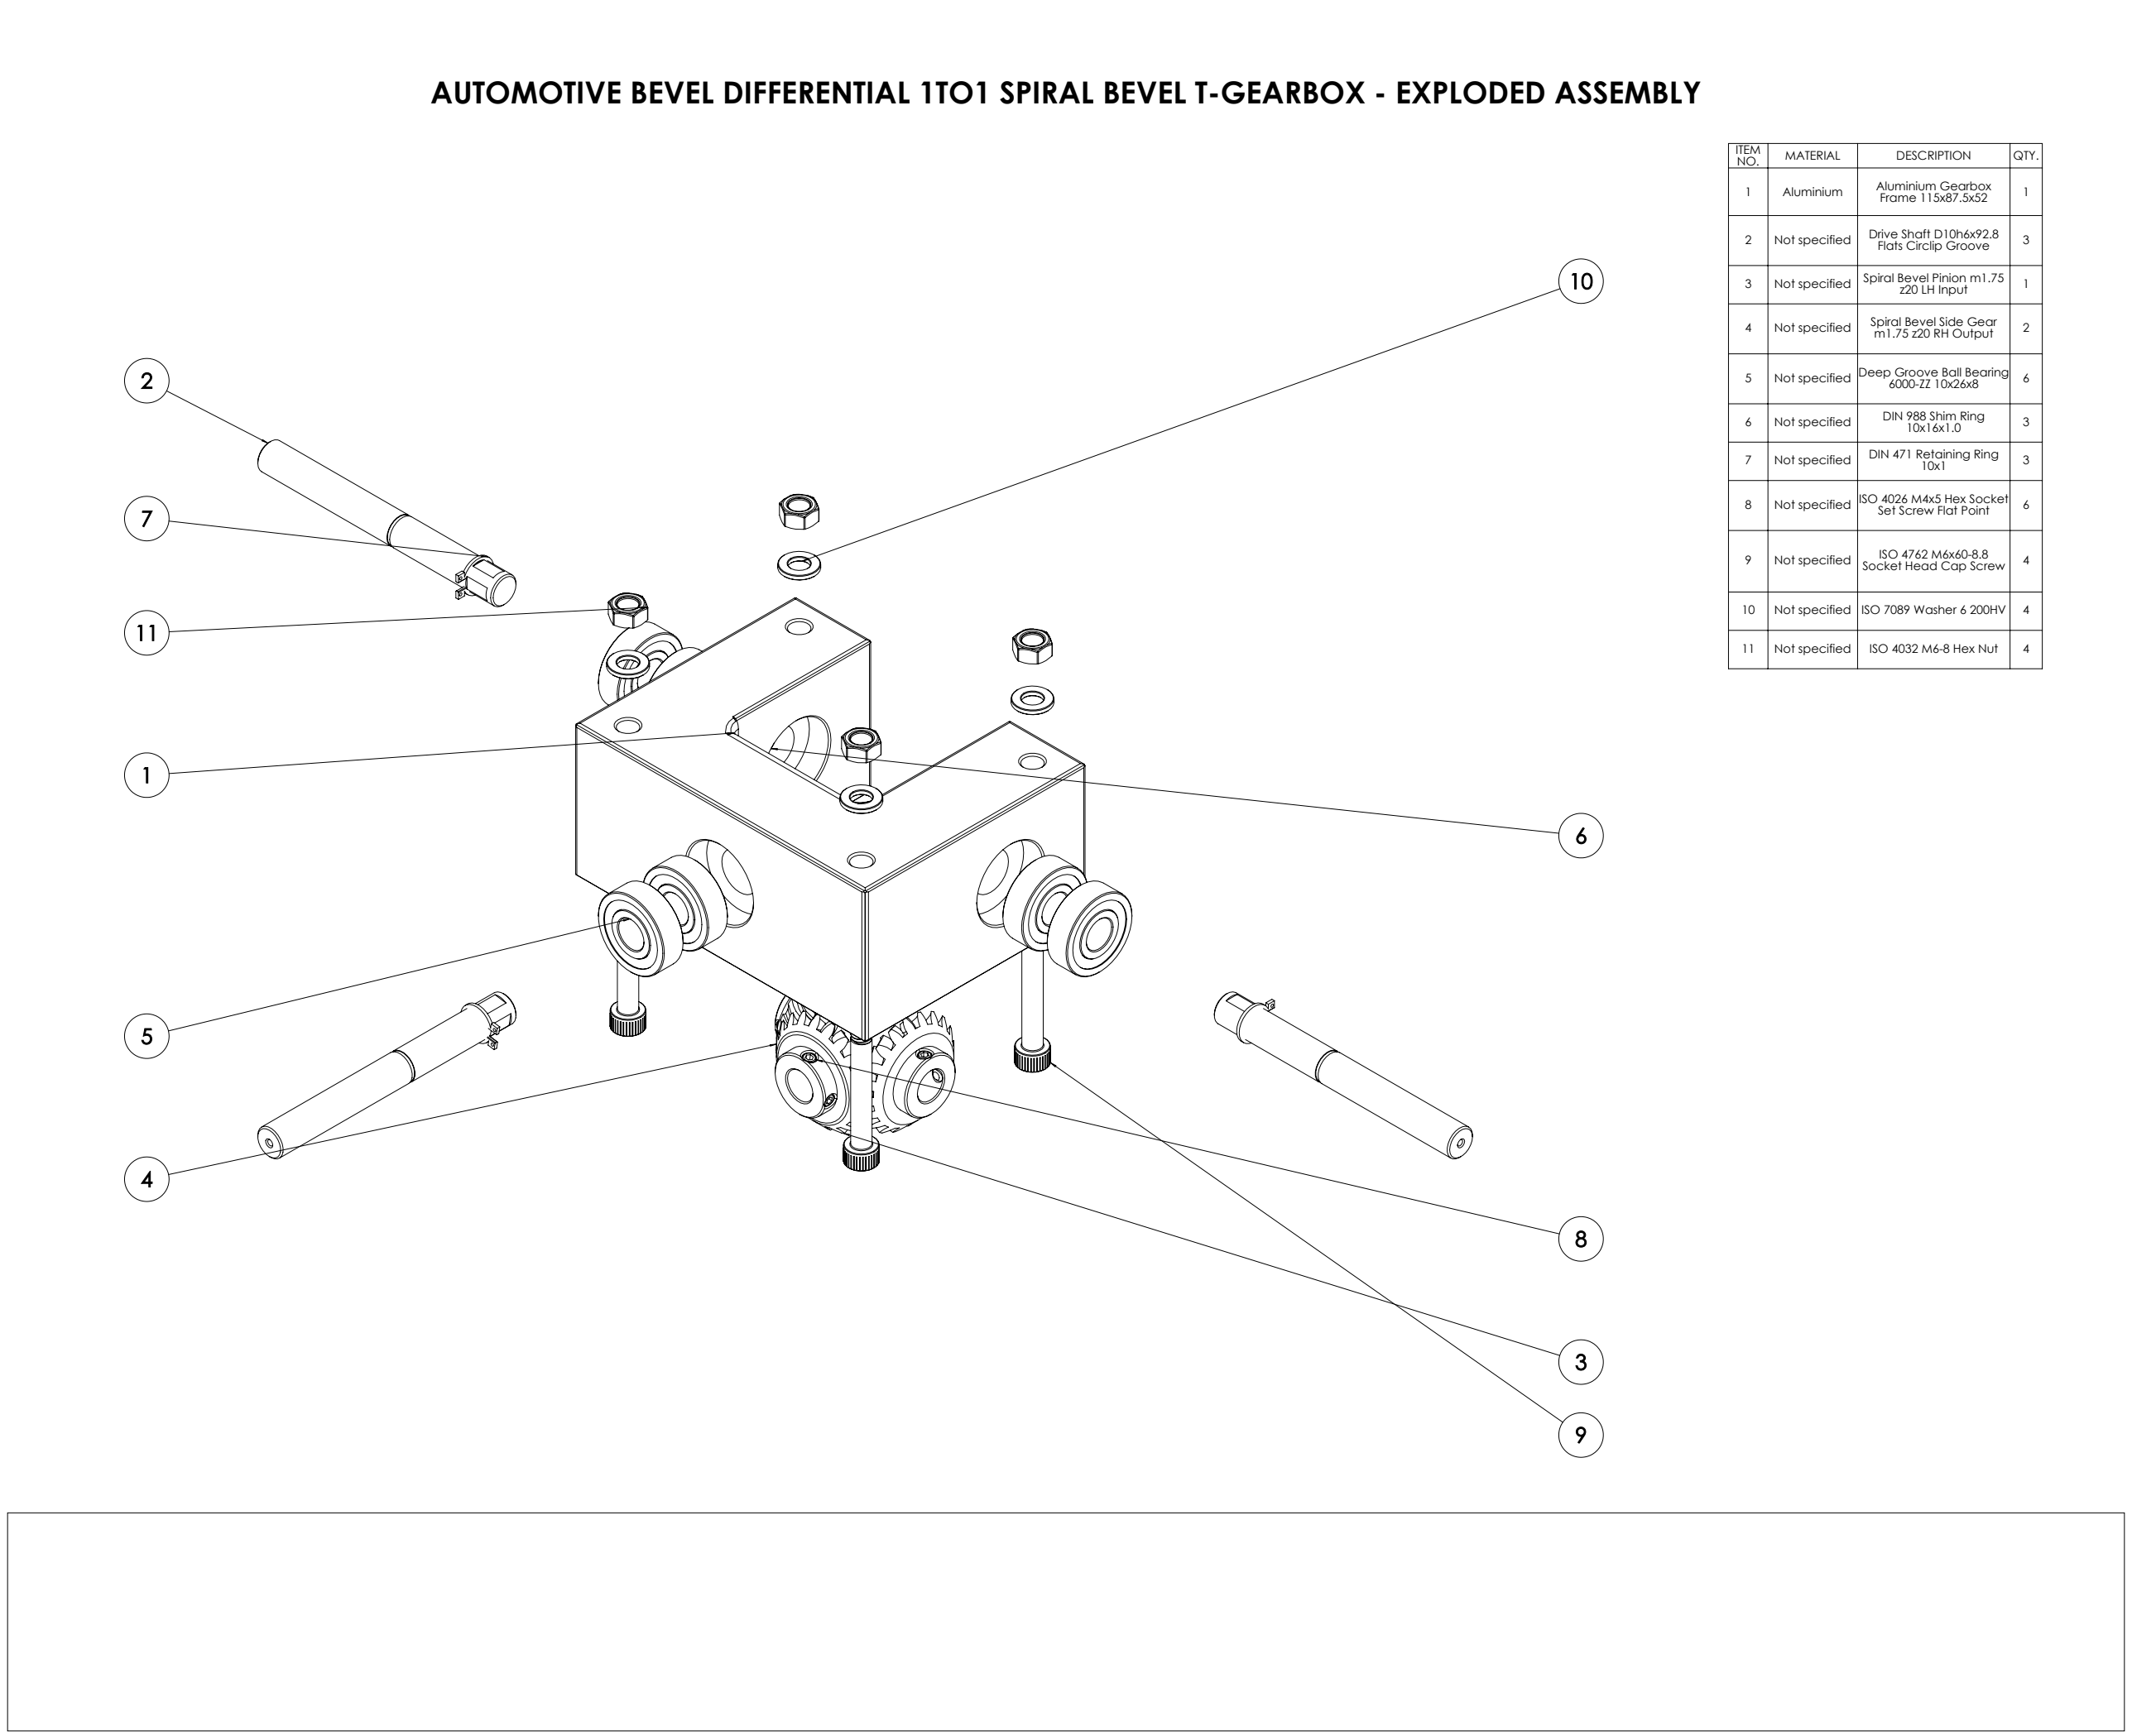
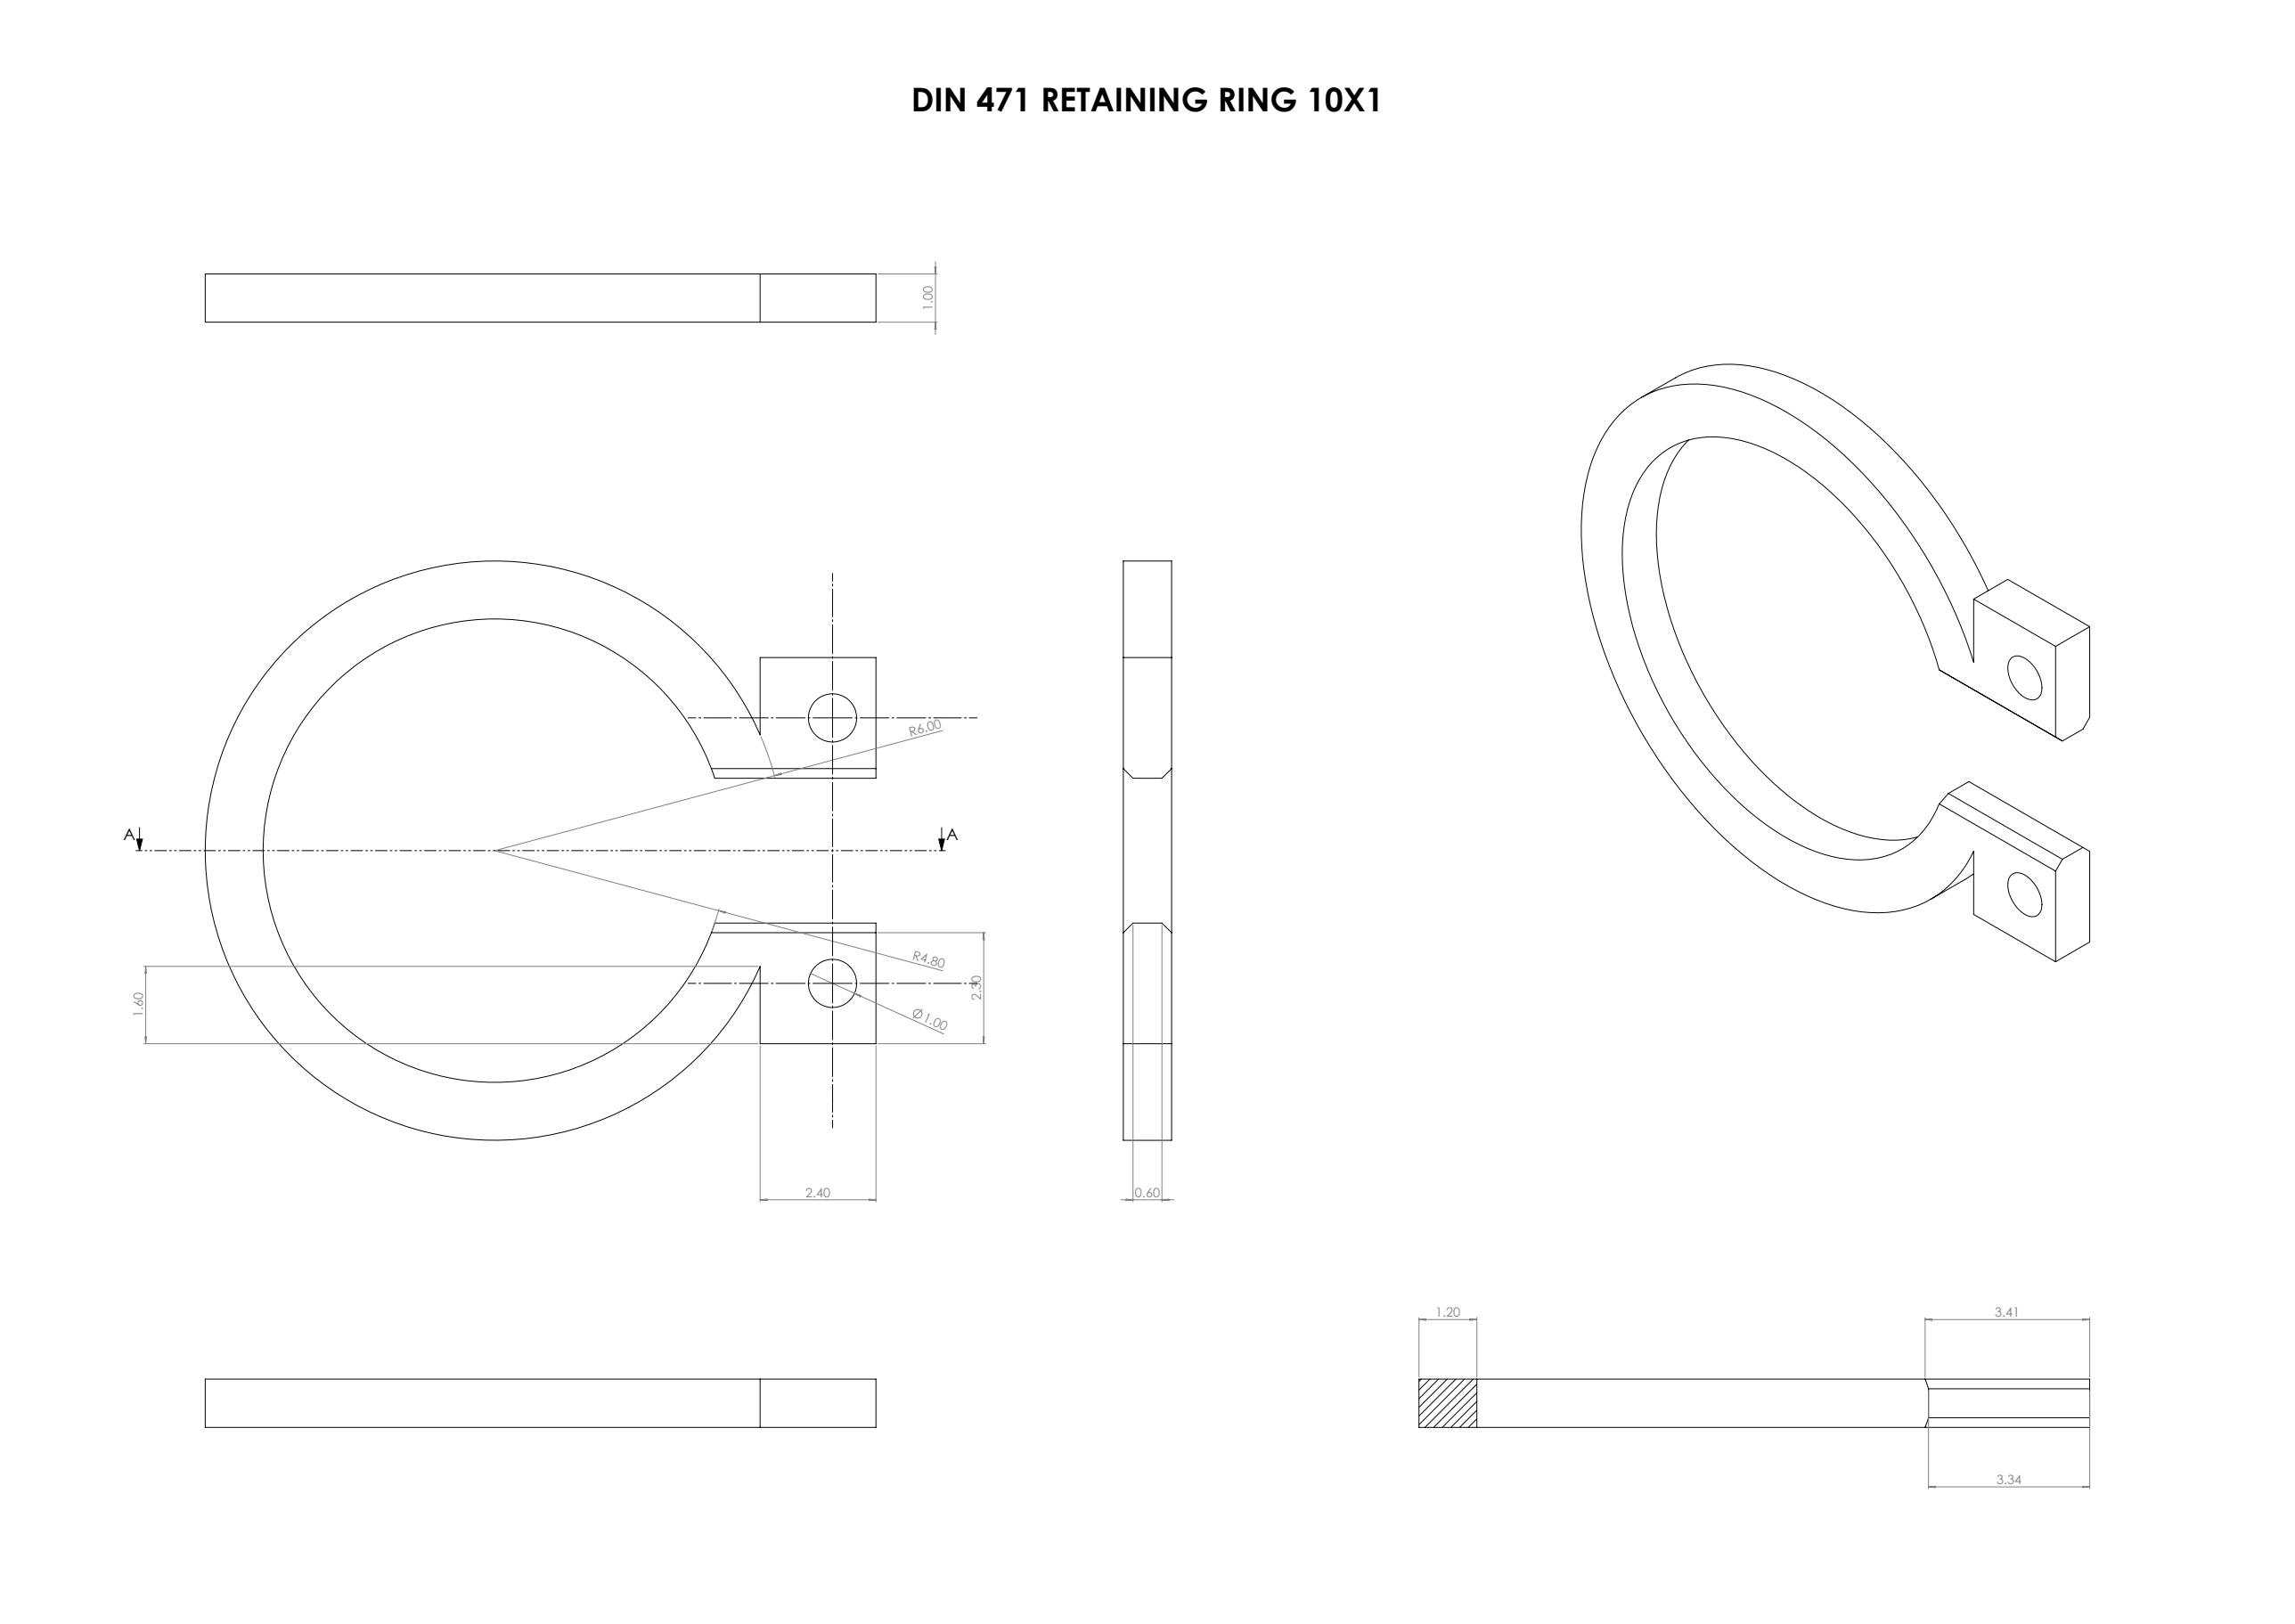
ISO-10303-21;
HEADER;
/* Generated by software containing ST-Developer
 * from STEP Tools, Inc. (www.steptools.com) 
 */

FILE_DESCRIPTION(
/* description */ (''),
/* implementation_level */ '2;1');

FILE_NAME(
/* name */ 
'MAS-358',
/* time_stamp */ '2026-10-22T00:21:42-07:00',
/* author */ (''),
/* organization */ (''),
/* preprocessor_version */ 'ST-DEVELOPER v20.2',
/* originating_system */ 'Autodesk Translation Framework v15.15.0.0',
/* authorisation */ '');

FILE_SCHEMA (('AUTOMOTIVE_DESIGN { 1 0 10303 214 3 1 1 }'));
ENDSEC;

DATA;
#10=MECHANICAL_DESIGN_GEOMETRIC_PRESENTATION_REPRESENTATION('',(#205,#206,
#207,#208,#209,#210,#211,#212,#213,#214,#215),#31638);
#11=ITEM_DEFINED_TRANSFORMATION($,$,#12614,#13583);
#12=ITEM_DEFINED_TRANSFORMATION($,$,#12865,#13584);
#13=ITEM_DEFINED_TRANSFORMATION($,$,#12776,#13585);
#14=ITEM_DEFINED_TRANSFORMATION($,$,#12900,#13586);
#15=ITEM_DEFINED_TRANSFORMATION($,$,#12986,#13587);
#16=ITEM_DEFINED_TRANSFORMATION($,$,#13096,#13588);
#17=ITEM_DEFINED_TRANSFORMATION($,$,#13105,#13589);
#18=ITEM_DEFINED_TRANSFORMATION($,$,#13136,#13590);
#19=ITEM_DEFINED_TRANSFORMATION($,$,#13175,#13591);
#20=ITEM_DEFINED_TRANSFORMATION($,$,#13515,#13592);
#21=ITEM_DEFINED_TRANSFORMATION($,$,#13535,#13593);
#22=ITEM_DEFINED_TRANSFORMATION($,$,#12865,#13594);
#23=ITEM_DEFINED_TRANSFORMATION($,$,#12865,#13595);
#24=ITEM_DEFINED_TRANSFORMATION($,$,#12900,#13596);
#25=ITEM_DEFINED_TRANSFORMATION($,$,#12986,#13597);
#26=ITEM_DEFINED_TRANSFORMATION($,$,#12986,#13598);
#27=ITEM_DEFINED_TRANSFORMATION($,$,#12986,#13599);
#28=ITEM_DEFINED_TRANSFORMATION($,$,#12986,#13600);
#29=ITEM_DEFINED_TRANSFORMATION($,$,#12986,#13601);
#30=ITEM_DEFINED_TRANSFORMATION($,$,#13096,#13602);
#31=ITEM_DEFINED_TRANSFORMATION($,$,#13096,#13603);
#32=ITEM_DEFINED_TRANSFORMATION($,$,#13105,#13604);
#33=ITEM_DEFINED_TRANSFORMATION($,$,#13105,#13605);
#34=ITEM_DEFINED_TRANSFORMATION($,$,#13136,#13606);
#35=ITEM_DEFINED_TRANSFORMATION($,$,#13136,#13607);
#36=ITEM_DEFINED_TRANSFORMATION($,$,#13136,#13608);
#37=ITEM_DEFINED_TRANSFORMATION($,$,#13136,#13609);
#38=ITEM_DEFINED_TRANSFORMATION($,$,#13136,#13610);
#39=ITEM_DEFINED_TRANSFORMATION($,$,#13175,#13611);
#40=ITEM_DEFINED_TRANSFORMATION($,$,#13175,#13612);
#41=ITEM_DEFINED_TRANSFORMATION($,$,#13175,#13613);
#42=ITEM_DEFINED_TRANSFORMATION($,$,#13515,#13614);
#43=ITEM_DEFINED_TRANSFORMATION($,$,#13515,#13615);
#44=ITEM_DEFINED_TRANSFORMATION($,$,#13515,#13616);
#45=ITEM_DEFINED_TRANSFORMATION($,$,#13535,#13617);
#46=ITEM_DEFINED_TRANSFORMATION($,$,#13535,#13618);
#47=ITEM_DEFINED_TRANSFORMATION($,$,#13535,#13619);
#48=(
REPRESENTATION_RELATIONSHIP($,$,#31705,#31704)
REPRESENTATION_RELATIONSHIP_WITH_TRANSFORMATION(#11)
SHAPE_REPRESENTATION_RELATIONSHIP()
);
#49=(
REPRESENTATION_RELATIONSHIP($,$,#31707,#31704)
REPRESENTATION_RELATIONSHIP_WITH_TRANSFORMATION(#12)
SHAPE_REPRESENTATION_RELATIONSHIP()
);
#50=(
REPRESENTATION_RELATIONSHIP($,$,#31706,#31704)
REPRESENTATION_RELATIONSHIP_WITH_TRANSFORMATION(#13)
SHAPE_REPRESENTATION_RELATIONSHIP()
);
#51=(
REPRESENTATION_RELATIONSHIP($,$,#31708,#31704)
REPRESENTATION_RELATIONSHIP_WITH_TRANSFORMATION(#14)
SHAPE_REPRESENTATION_RELATIONSHIP()
);
#52=(
REPRESENTATION_RELATIONSHIP($,$,#31709,#31704)
REPRESENTATION_RELATIONSHIP_WITH_TRANSFORMATION(#15)
SHAPE_REPRESENTATION_RELATIONSHIP()
);
#53=(
REPRESENTATION_RELATIONSHIP($,$,#31710,#31704)
REPRESENTATION_RELATIONSHIP_WITH_TRANSFORMATION(#16)
SHAPE_REPRESENTATION_RELATIONSHIP()
);
#54=(
REPRESENTATION_RELATIONSHIP($,$,#31711,#31704)
REPRESENTATION_RELATIONSHIP_WITH_TRANSFORMATION(#17)
SHAPE_REPRESENTATION_RELATIONSHIP()
);
#55=(
REPRESENTATION_RELATIONSHIP($,$,#31712,#31704)
REPRESENTATION_RELATIONSHIP_WITH_TRANSFORMATION(#18)
SHAPE_REPRESENTATION_RELATIONSHIP()
);
#56=(
REPRESENTATION_RELATIONSHIP($,$,#31713,#31704)
REPRESENTATION_RELATIONSHIP_WITH_TRANSFORMATION(#19)
SHAPE_REPRESENTATION_RELATIONSHIP()
);
#57=(
REPRESENTATION_RELATIONSHIP($,$,#31714,#31704)
REPRESENTATION_RELATIONSHIP_WITH_TRANSFORMATION(#20)
SHAPE_REPRESENTATION_RELATIONSHIP()
);
#58=(
REPRESENTATION_RELATIONSHIP($,$,#31715,#31704)
REPRESENTATION_RELATIONSHIP_WITH_TRANSFORMATION(#21)
SHAPE_REPRESENTATION_RELATIONSHIP()
);
#59=(
REPRESENTATION_RELATIONSHIP($,$,#31707,#31704)
REPRESENTATION_RELATIONSHIP_WITH_TRANSFORMATION(#22)
SHAPE_REPRESENTATION_RELATIONSHIP()
);
#60=(
REPRESENTATION_RELATIONSHIP($,$,#31707,#31704)
REPRESENTATION_RELATIONSHIP_WITH_TRANSFORMATION(#23)
SHAPE_REPRESENTATION_RELATIONSHIP()
);
#61=(
REPRESENTATION_RELATIONSHIP($,$,#31708,#31704)
REPRESENTATION_RELATIONSHIP_WITH_TRANSFORMATION(#24)
SHAPE_REPRESENTATION_RELATIONSHIP()
);
#62=(
REPRESENTATION_RELATIONSHIP($,$,#31709,#31704)
REPRESENTATION_RELATIONSHIP_WITH_TRANSFORMATION(#25)
SHAPE_REPRESENTATION_RELATIONSHIP()
);
#63=(
REPRESENTATION_RELATIONSHIP($,$,#31709,#31704)
REPRESENTATION_RELATIONSHIP_WITH_TRANSFORMATION(#26)
SHAPE_REPRESENTATION_RELATIONSHIP()
);
#64=(
REPRESENTATION_RELATIONSHIP($,$,#31709,#31704)
REPRESENTATION_RELATIONSHIP_WITH_TRANSFORMATION(#27)
SHAPE_REPRESENTATION_RELATIONSHIP()
);
#65=(
REPRESENTATION_RELATIONSHIP($,$,#31709,#31704)
REPRESENTATION_RELATIONSHIP_WITH_TRANSFORMATION(#28)
SHAPE_REPRESENTATION_RELATIONSHIP()
);
#66=(
REPRESENTATION_RELATIONSHIP($,$,#31709,#31704)
REPRESENTATION_RELATIONSHIP_WITH_TRANSFORMATION(#29)
SHAPE_REPRESENTATION_RELATIONSHIP()
);
#67=(
REPRESENTATION_RELATIONSHIP($,$,#31710,#31704)
REPRESENTATION_RELATIONSHIP_WITH_TRANSFORMATION(#30)
SHAPE_REPRESENTATION_RELATIONSHIP()
);
#68=(
REPRESENTATION_RELATIONSHIP($,$,#31710,#31704)
REPRESENTATION_RELATIONSHIP_WITH_TRANSFORMATION(#31)
SHAPE_REPRESENTATION_RELATIONSHIP()
);
#69=(
REPRESENTATION_RELATIONSHIP($,$,#31711,#31704)
REPRESENTATION_RELATIONSHIP_WITH_TRANSFORMATION(#32)
SHAPE_REPRESENTATION_RELATIONSHIP()
);
#70=(
REPRESENTATION_RELATIONSHIP($,$,#31711,#31704)
REPRESENTATION_RELATIONSHIP_WITH_TRANSFORMATION(#33)
SHAPE_REPRESENTATION_RELATIONSHIP()
);
#71=(
REPRESENTATION_RELATIONSHIP($,$,#31712,#31704)
REPRESENTATION_RELATIONSHIP_WITH_TRANSFORMATION(#34)
SHAPE_REPRESENTATION_RELATIONSHIP()
);
#72=(
REPRESENTATION_RELATIONSHIP($,$,#31712,#31704)
REPRESENTATION_RELATIONSHIP_WITH_TRANSFORMATION(#35)
SHAPE_REPRESENTATION_RELATIONSHIP()
);
#73=(
REPRESENTATION_RELATIONSHIP($,$,#31712,#31704)
REPRESENTATION_RELATIONSHIP_WITH_TRANSFORMATION(#36)
SHAPE_REPRESENTATION_RELATIONSHIP()
);
#74=(
REPRESENTATION_RELATIONSHIP($,$,#31712,#31704)
REPRESENTATION_RELATIONSHIP_WITH_TRANSFORMATION(#37)
SHAPE_REPRESENTATION_RELATIONSHIP()
);
#75=(
REPRESENTATION_RELATIONSHIP($,$,#31712,#31704)
REPRESENTATION_RELATIONSHIP_WITH_TRANSFORMATION(#38)
SHAPE_REPRESENTATION_RELATIONSHIP()
);
#76=(
REPRESENTATION_RELATIONSHIP($,$,#31713,#31704)
REPRESENTATION_RELATIONSHIP_WITH_TRANSFORMATION(#39)
SHAPE_REPRESENTATION_RELATIONSHIP()
);
#77=(
REPRESENTATION_RELATIONSHIP($,$,#31713,#31704)
REPRESENTATION_RELATIONSHIP_WITH_TRANSFORMATION(#40)
SHAPE_REPRESENTATION_RELATIONSHIP()
);
#78=(
REPRESENTATION_RELATIONSHIP($,$,#31713,#31704)
REPRESENTATION_RELATIONSHIP_WITH_TRANSFORMATION(#41)
SHAPE_REPRESENTATION_RELATIONSHIP()
);
#79=(
REPRESENTATION_RELATIONSHIP($,$,#31714,#31704)
REPRESENTATION_RELATIONSHIP_WITH_TRANSFORMATION(#42)
SHAPE_REPRESENTATION_RELATIONSHIP()
);
#80=(
REPRESENTATION_RELATIONSHIP($,$,#31714,#31704)
REPRESENTATION_RELATIONSHIP_WITH_TRANSFORMATION(#43)
SHAPE_REPRESENTATION_RELATIONSHIP()
);
#81=(
REPRESENTATION_RELATIONSHIP($,$,#31714,#31704)
REPRESENTATION_RELATIONSHIP_WITH_TRANSFORMATION(#44)
SHAPE_REPRESENTATION_RELATIONSHIP()
);
#82=(
REPRESENTATION_RELATIONSHIP($,$,#31715,#31704)
REPRESENTATION_RELATIONSHIP_WITH_TRANSFORMATION(#45)
SHAPE_REPRESENTATION_RELATIONSHIP()
);
#83=(
REPRESENTATION_RELATIONSHIP($,$,#31715,#31704)
REPRESENTATION_RELATIONSHIP_WITH_TRANSFORMATION(#46)
SHAPE_REPRESENTATION_RELATIONSHIP()
);
#84=(
REPRESENTATION_RELATIONSHIP($,$,#31715,#31704)
REPRESENTATION_RELATIONSHIP_WITH_TRANSFORMATION(#47)
SHAPE_REPRESENTATION_RELATIONSHIP()
);
#85=CONTEXT_DEPENDENT_SHAPE_REPRESENTATION(#48,#31667);
#86=CONTEXT_DEPENDENT_SHAPE_REPRESENTATION(#49,#31668);
#87=CONTEXT_DEPENDENT_SHAPE_REPRESENTATION(#50,#31669);
#88=CONTEXT_DEPENDENT_SHAPE_REPRESENTATION(#51,#31670);
#89=CONTEXT_DEPENDENT_SHAPE_REPRESENTATION(#52,#31671);
#90=CONTEXT_DEPENDENT_SHAPE_REPRESENTATION(#53,#31672);
#91=CONTEXT_DEPENDENT_SHAPE_REPRESENTATION(#54,#31673);
#92=CONTEXT_DEPENDENT_SHAPE_REPRESENTATION(#55,#31674);
#93=CONTEXT_DEPENDENT_SHAPE_REPRESENTATION(#56,#31675);
#94=CONTEXT_DEPENDENT_SHAPE_REPRESENTATION(#57,#31676);
#95=CONTEXT_DEPENDENT_SHAPE_REPRESENTATION(#58,#31677);
#96=CONTEXT_DEPENDENT_SHAPE_REPRESENTATION(#59,#31678);
#97=CONTEXT_DEPENDENT_SHAPE_REPRESENTATION(#60,#31679);
#98=CONTEXT_DEPENDENT_SHAPE_REPRESENTATION(#61,#31680);
#99=CONTEXT_DEPENDENT_SHAPE_REPRESENTATION(#62,#31681);
#100=CONTEXT_DEPENDENT_SHAPE_REPRESENTATION(#63,#31682);
#101=CONTEXT_DEPENDENT_SHAPE_REPRESENTATION(#64,#31683);
#102=CONTEXT_DEPENDENT_SHAPE_REPRESENTATION(#65,#31684);
#103=CONTEXT_DEPENDENT_SHAPE_REPRESENTATION(#66,#31685);
#104=CONTEXT_DEPENDENT_SHAPE_REPRESENTATION(#67,#31686);
#105=CONTEXT_DEPENDENT_SHAPE_REPRESENTATION(#68,#31687);
#106=CONTEXT_DEPENDENT_SHAPE_REPRESENTATION(#69,#31688);
#107=CONTEXT_DEPENDENT_SHAPE_REPRESENTATION(#70,#31689);
#108=CONTEXT_DEPENDENT_SHAPE_REPRESENTATION(#71,#31690);
#109=CONTEXT_DEPENDENT_SHAPE_REPRESENTATION(#72,#31691);
#110=CONTEXT_DEPENDENT_SHAPE_REPRESENTATION(#73,#31692);
#111=CONTEXT_DEPENDENT_SHAPE_REPRESENTATION(#74,#31693);
#112=CONTEXT_DEPENDENT_SHAPE_REPRESENTATION(#75,#31694);
#113=CONTEXT_DEPENDENT_SHAPE_REPRESENTATION(#76,#31695);
#114=CONTEXT_DEPENDENT_SHAPE_REPRESENTATION(#77,#31696);
#115=CONTEXT_DEPENDENT_SHAPE_REPRESENTATION(#78,#31697);
#116=CONTEXT_DEPENDENT_SHAPE_REPRESENTATION(#79,#31698);
#117=CONTEXT_DEPENDENT_SHAPE_REPRESENTATION(#80,#31699);
#118=CONTEXT_DEPENDENT_SHAPE_REPRESENTATION(#81,#31700);
#119=CONTEXT_DEPENDENT_SHAPE_REPRESENTATION(#82,#31701);
#120=CONTEXT_DEPENDENT_SHAPE_REPRESENTATION(#83,#31702);
#121=CONTEXT_DEPENDENT_SHAPE_REPRESENTATION(#84,#31703);
#122=NEXT_ASSEMBLY_USAGE_OCCURRENCE(
'01_Aluminium_Gearbox_Frame_115x87.5x52:1',
'01_Aluminium_Gearbox_Frame_115x87.5x52:1',
'01_Aluminium_Gearbox_Frame_115x87.5x52:1',#31717,#31718,
'01_Aluminium_Gearbox_Frame_115x87.5x52:1');
#123=NEXT_ASSEMBLY_USAGE_OCCURRENCE(
'02_Drive_Shaft_D10h6x92.8_Flats_Circlip_Groove:1',
'02_Drive_Shaft_D10h6x92.8_Flats_Circlip_Groove:1',
'02_Drive_Shaft_D10h6x92.8_Flats_Circlip_Groove:1',#31717,#31720,
'02_Drive_Shaft_D10h6x92.8_Flats_Circlip_Groove:1');
#124=NEXT_ASSEMBLY_USAGE_OCCURRENCE(
'03_Spiral_Bevel_Pinion_m1.75_z20_LH_Input:1',
'03_Spiral_Bevel_Pinion_m1.75_z20_LH_Input:1',
'03_Spiral_Bevel_Pinion_m1.75_z20_LH_Input:1',#31717,#31719,
'03_Spiral_Bevel_Pinion_m1.75_z20_LH_Input:1');
#125=NEXT_ASSEMBLY_USAGE_OCCURRENCE(
'04_Spiral_Bevel_Side_Gear_m1.75_z20_RH_Output:1',
'04_Spiral_Bevel_Side_Gear_m1.75_z20_RH_Output:1',
'04_Spiral_Bevel_Side_Gear_m1.75_z20_RH_Output:1',#31717,#31721,
'04_Spiral_Bevel_Side_Gear_m1.75_z20_RH_Output:1');
#126=NEXT_ASSEMBLY_USAGE_OCCURRENCE(
'05_Deep_Groove_Ball_Bearing_6000-ZZ_10x26x8:1',
'05_Deep_Groove_Ball_Bearing_6000-ZZ_10x26x8:1',
'05_Deep_Groove_Ball_Bearing_6000-ZZ_10x26x8:1',#31717,#31722,
'05_Deep_Groove_Ball_Bearing_6000-ZZ_10x26x8:1');
#127=NEXT_ASSEMBLY_USAGE_OCCURRENCE('06_DIN_988_Shim_Ring_10x16x1.0:1',
'06_DIN_988_Shim_Ring_10x16x1.0:1','06_DIN_988_Shim_Ring_10x16x1.0:1',#31717,
#31723,'06_DIN_988_Shim_Ring_10x16x1.0:1');
#128=NEXT_ASSEMBLY_USAGE_OCCURRENCE('07_DIN_471_Retaining_Ring_10x1:1',
'07_DIN_471_Retaining_Ring_10x1:1','07_DIN_471_Retaining_Ring_10x1:1',#31717,
#31724,'07_DIN_471_Retaining_Ring_10x1:1');
#129=NEXT_ASSEMBLY_USAGE_OCCURRENCE(
'08_ISO_4026_M4x5_Hex_Socket_Set_Screw_Flat_Point:1',
'08_ISO_4026_M4x5_Hex_Socket_Set_Screw_Flat_Point:1',
'08_ISO_4026_M4x5_Hex_Socket_Set_Screw_Flat_Point:1',#31717,#31725,
'08_ISO_4026_M4x5_Hex_Socket_Set_Screw_Flat_Point:1');
#130=NEXT_ASSEMBLY_USAGE_OCCURRENCE(
'09_ISO_4762_M6x60-8.8_Socket_Head_Cap_Screw:1',
'09_ISO_4762_M6x60-8.8_Socket_Head_Cap_Screw:1',
'09_ISO_4762_M6x60-8.8_Socket_Head_Cap_Screw:1',#31717,#31726,
'09_ISO_4762_M6x60-8.8_Socket_Head_Cap_Screw:1');
#131=NEXT_ASSEMBLY_USAGE_OCCURRENCE('10_ISO_7089_Washer_6_200HV:1',
'10_ISO_7089_Washer_6_200HV:1','10_ISO_7089_Washer_6_200HV:1',#31717,#31727,
'10_ISO_7089_Washer_6_200HV:1');
#132=NEXT_ASSEMBLY_USAGE_OCCURRENCE('11_ISO_4032_M6-8_Hex_Nut:1',
'11_ISO_4032_M6-8_Hex_Nut:1','11_ISO_4032_M6-8_Hex_Nut:1',#31717,#31728,
'11_ISO_4032_M6-8_Hex_Nut:1');
#133=NEXT_ASSEMBLY_USAGE_OCCURRENCE(
'02_Drive_Shaft_D10h6x92.8_Flats_Circlip_Groove:2',
'02_Drive_Shaft_D10h6x92.8_Flats_Circlip_Groove:2',
'02_Drive_Shaft_D10h6x92.8_Flats_Circlip_Groove:2',#31717,#31720,
'02_Drive_Shaft_D10h6x92.8_Flats_Circlip_Groove:2');
#134=NEXT_ASSEMBLY_USAGE_OCCURRENCE(
'02_Drive_Shaft_D10h6x92.8_Flats_Circlip_Groove:3',
'02_Drive_Shaft_D10h6x92.8_Flats_Circlip_Groove:3',
'02_Drive_Shaft_D10h6x92.8_Flats_Circlip_Groove:3',#31717,#31720,
'02_Drive_Shaft_D10h6x92.8_Flats_Circlip_Groove:3');
#135=NEXT_ASSEMBLY_USAGE_OCCURRENCE(
'04_Spiral_Bevel_Side_Gear_m1.75_z20_RH_Output:2',
'04_Spiral_Bevel_Side_Gear_m1.75_z20_RH_Output:2',
'04_Spiral_Bevel_Side_Gear_m1.75_z20_RH_Output:2',#31717,#31721,
'04_Spiral_Bevel_Side_Gear_m1.75_z20_RH_Output:2');
#136=NEXT_ASSEMBLY_USAGE_OCCURRENCE(
'05_Deep_Groove_Ball_Bearing_6000-ZZ_10x26x8:2',
'05_Deep_Groove_Ball_Bearing_6000-ZZ_10x26x8:2',
'05_Deep_Groove_Ball_Bearing_6000-ZZ_10x26x8:2',#31717,#31722,
'05_Deep_Groove_Ball_Bearing_6000-ZZ_10x26x8:2');
#137=NEXT_ASSEMBLY_USAGE_OCCURRENCE(
'05_Deep_Groove_Ball_Bearing_6000-ZZ_10x26x8:3',
'05_Deep_Groove_Ball_Bearing_6000-ZZ_10x26x8:3',
'05_Deep_Groove_Ball_Bearing_6000-ZZ_10x26x8:3',#31717,#31722,
'05_Deep_Groove_Ball_Bearing_6000-ZZ_10x26x8:3');
#138=NEXT_ASSEMBLY_USAGE_OCCURRENCE(
'05_Deep_Groove_Ball_Bearing_6000-ZZ_10x26x8:4',
'05_Deep_Groove_Ball_Bearing_6000-ZZ_10x26x8:4',
'05_Deep_Groove_Ball_Bearing_6000-ZZ_10x26x8:4',#31717,#31722,
'05_Deep_Groove_Ball_Bearing_6000-ZZ_10x26x8:4');
#139=NEXT_ASSEMBLY_USAGE_OCCURRENCE(
'05_Deep_Groove_Ball_Bearing_6000-ZZ_10x26x8:5',
'05_Deep_Groove_Ball_Bearing_6000-ZZ_10x26x8:5',
'05_Deep_Groove_Ball_Bearing_6000-ZZ_10x26x8:5',#31717,#31722,
'05_Deep_Groove_Ball_Bearing_6000-ZZ_10x26x8:5');
#140=NEXT_ASSEMBLY_USAGE_OCCURRENCE(
'05_Deep_Groove_Ball_Bearing_6000-ZZ_10x26x8:6',
'05_Deep_Groove_Ball_Bearing_6000-ZZ_10x26x8:6',
'05_Deep_Groove_Ball_Bearing_6000-ZZ_10x26x8:6',#31717,#31722,
'05_Deep_Groove_Ball_Bearing_6000-ZZ_10x26x8:6');
#141=NEXT_ASSEMBLY_USAGE_OCCURRENCE('06_DIN_988_Shim_Ring_10x16x1.0:2',
'06_DIN_988_Shim_Ring_10x16x1.0:2','06_DIN_988_Shim_Ring_10x16x1.0:2',#31717,
#31723,'06_DIN_988_Shim_Ring_10x16x1.0:2');
#142=NEXT_ASSEMBLY_USAGE_OCCURRENCE('06_DIN_988_Shim_Ring_10x16x1.0:3',
'06_DIN_988_Shim_Ring_10x16x1.0:3','06_DIN_988_Shim_Ring_10x16x1.0:3',#31717,
#31723,'06_DIN_988_Shim_Ring_10x16x1.0:3');
#143=NEXT_ASSEMBLY_USAGE_OCCURRENCE('07_DIN_471_Retaining_Ring_10x1:2',
'07_DIN_471_Retaining_Ring_10x1:2','07_DIN_471_Retaining_Ring_10x1:2',#31717,
#31724,'07_DIN_471_Retaining_Ring_10x1:2');
#144=NEXT_ASSEMBLY_USAGE_OCCURRENCE('07_DIN_471_Retaining_Ring_10x1:3',
'07_DIN_471_Retaining_Ring_10x1:3','07_DIN_471_Retaining_Ring_10x1:3',#31717,
#31724,'07_DIN_471_Retaining_Ring_10x1:3');
#145=NEXT_ASSEMBLY_USAGE_OCCURRENCE(
'08_ISO_4026_M4x5_Hex_Socket_Set_Screw_Flat_Point:2',
'08_ISO_4026_M4x5_Hex_Socket_Set_Screw_Flat_Point:2',
'08_ISO_4026_M4x5_Hex_Socket_Set_Screw_Flat_Point:2',#31717,#31725,
'08_ISO_4026_M4x5_Hex_Socket_Set_Screw_Flat_Point:2');
#146=NEXT_ASSEMBLY_USAGE_OCCURRENCE(
'08_ISO_4026_M4x5_Hex_Socket_Set_Screw_Flat_Point:3',
'08_ISO_4026_M4x5_Hex_Socket_Set_Screw_Flat_Point:3',
'08_ISO_4026_M4x5_Hex_Socket_Set_Screw_Flat_Point:3',#31717,#31725,
'08_ISO_4026_M4x5_Hex_Socket_Set_Screw_Flat_Point:3');
#147=NEXT_ASSEMBLY_USAGE_OCCURRENCE(
'08_ISO_4026_M4x5_Hex_Socket_Set_Screw_Flat_Point:4',
'08_ISO_4026_M4x5_Hex_Socket_Set_Screw_Flat_Point:4',
'08_ISO_4026_M4x5_Hex_Socket_Set_Screw_Flat_Point:4',#31717,#31725,
'08_ISO_4026_M4x5_Hex_Socket_Set_Screw_Flat_Point:4');
#148=NEXT_ASSEMBLY_USAGE_OCCURRENCE(
'08_ISO_4026_M4x5_Hex_Socket_Set_Screw_Flat_Point:5',
'08_ISO_4026_M4x5_Hex_Socket_Set_Screw_Flat_Point:5',
'08_ISO_4026_M4x5_Hex_Socket_Set_Screw_Flat_Point:5',#31717,#31725,
'08_ISO_4026_M4x5_Hex_Socket_Set_Screw_Flat_Point:5');
#149=NEXT_ASSEMBLY_USAGE_OCCURRENCE(
'08_ISO_4026_M4x5_Hex_Socket_Set_Screw_Flat_Point:6',
'08_ISO_4026_M4x5_Hex_Socket_Set_Screw_Flat_Point:6',
'08_ISO_4026_M4x5_Hex_Socket_Set_Screw_Flat_Point:6',#31717,#31725,
'08_ISO_4026_M4x5_Hex_Socket_Set_Screw_Flat_Point:6');
#150=NEXT_ASSEMBLY_USAGE_OCCURRENCE(
'09_ISO_4762_M6x60-8.8_Socket_Head_Cap_Screw:2',
'09_ISO_4762_M6x60-8.8_Socket_Head_Cap_Screw:2',
'09_ISO_4762_M6x60-8.8_Socket_Head_Cap_Screw:2',#31717,#31726,
'09_ISO_4762_M6x60-8.8_Socket_Head_Cap_Screw:2');
#151=NEXT_ASSEMBLY_USAGE_OCCURRENCE(
'09_ISO_4762_M6x60-8.8_Socket_Head_Cap_Screw:3',
'09_ISO_4762_M6x60-8.8_Socket_Head_Cap_Screw:3',
'09_ISO_4762_M6x60-8.8_Socket_Head_Cap_Screw:3',#31717,#31726,
'09_ISO_4762_M6x60-8.8_Socket_Head_Cap_Screw:3');
#152=NEXT_ASSEMBLY_USAGE_OCCURRENCE(
'09_ISO_4762_M6x60-8.8_Socket_Head_Cap_Screw:4',
'09_ISO_4762_M6x60-8.8_Socket_Head_Cap_Screw:4',
'09_ISO_4762_M6x60-8.8_Socket_Head_Cap_Screw:4',#31717,#31726,
'09_ISO_4762_M6x60-8.8_Socket_Head_Cap_Screw:4');
#153=NEXT_ASSEMBLY_USAGE_OCCURRENCE('10_ISO_7089_Washer_6_200HV:2',
'10_ISO_7089_Washer_6_200HV:2','10_ISO_7089_Washer_6_200HV:2',#31717,#31727,
'10_ISO_7089_Washer_6_200HV:2');
#154=NEXT_ASSEMBLY_USAGE_OCCURRENCE('10_ISO_7089_Washer_6_200HV:3',
'10_ISO_7089_Washer_6_200HV:3','10_ISO_7089_Washer_6_200HV:3',#31717,#31727,
'10_ISO_7089_Washer_6_200HV:3');
#155=NEXT_ASSEMBLY_USAGE_OCCURRENCE('10_ISO_7089_Washer_6_200HV:4',
'10_ISO_7089_Washer_6_200HV:4','10_ISO_7089_Washer_6_200HV:4',#31717,#31727,
'10_ISO_7089_Washer_6_200HV:4');
#156=NEXT_ASSEMBLY_USAGE_OCCURRENCE('11_ISO_4032_M6-8_Hex_Nut:2',
'11_ISO_4032_M6-8_Hex_Nut:2','11_ISO_4032_M6-8_Hex_Nut:2',#31717,#31728,
'11_ISO_4032_M6-8_Hex_Nut:2');
#157=NEXT_ASSEMBLY_USAGE_OCCURRENCE('11_ISO_4032_M6-8_Hex_Nut:3',
'11_ISO_4032_M6-8_Hex_Nut:3','11_ISO_4032_M6-8_Hex_Nut:3',#31717,#31728,
'11_ISO_4032_M6-8_Hex_Nut:3');
#158=NEXT_ASSEMBLY_USAGE_OCCURRENCE('11_ISO_4032_M6-8_Hex_Nut:4',
'11_ISO_4032_M6-8_Hex_Nut:4','11_ISO_4032_M6-8_Hex_Nut:4',#31717,#31728,
'11_ISO_4032_M6-8_Hex_Nut:4');
#159=(
BOUNDED_CURVE()
B_SPLINE_CURVE(2,(#31154,#31155,#31156),.UNSPECIFIED.,.F.,.F.)
B_SPLINE_CURVE_WITH_KNOTS((3,3),(0.0913980941282311,0.128154684519473),
 .UNSPECIFIED.)
CURVE()
GEOMETRIC_REPRESENTATION_ITEM()
RATIONAL_B_SPLINE_CURVE((1.009002117709,1.00952129238835,1.009002117709))
REPRESENTATION_ITEM('')
);
#160=(
BOUNDED_CURVE()
B_SPLINE_CURVE(2,(#31282,#31283,#31284),.UNSPECIFIED.,.F.,.F.)
B_SPLINE_CURVE_WITH_KNOTS((3,3),(0.0913980941282308,0.128154684519473),
 .UNSPECIFIED.)
CURVE()
GEOMETRIC_REPRESENTATION_ITEM()
RATIONAL_B_SPLINE_CURVE((1.009002117709,1.00952129238836,1.009002117709))
REPRESENTATION_ITEM('')
);
#161=(
BOUNDED_CURVE()
B_SPLINE_CURVE(2,(#31290,#31291,#31292),.UNSPECIFIED.,.F.,.F.)
B_SPLINE_CURVE_WITH_KNOTS((3,3),(0.0913980941282322,0.128154684519474),
 .UNSPECIFIED.)
CURVE()
GEOMETRIC_REPRESENTATION_ITEM()
RATIONAL_B_SPLINE_CURVE((1.009002117709,1.00952129238836,1.009002117709))
REPRESENTATION_ITEM('')
);
#162=(
BOUNDED_CURVE()
B_SPLINE_CURVE(2,(#31423,#31424,#31425),.UNSPECIFIED.,.F.,.F.)
B_SPLINE_CURVE_WITH_KNOTS((3,3),(0.0913980941282321,0.128154684519474),
 .UNSPECIFIED.)
CURVE()
GEOMETRIC_REPRESENTATION_ITEM()
RATIONAL_B_SPLINE_CURVE((1.009002117709,1.00952129238835,1.009002117709))
REPRESENTATION_ITEM('')
);
#163=(
BOUNDED_CURVE()
B_SPLINE_CURVE(2,(#31431,#31432,#31433),.UNSPECIFIED.,.F.,.F.)
B_SPLINE_CURVE_WITH_KNOTS((3,3),(0.0913980941282314,0.128154684519474),
 .UNSPECIFIED.)
CURVE()
GEOMETRIC_REPRESENTATION_ITEM()
RATIONAL_B_SPLINE_CURVE((1.00900211770901,1.00952129238836,1.00900211770901))
REPRESENTATION_ITEM('')
);
#164=(
BOUNDED_CURVE()
B_SPLINE_CURVE(2,(#31499,#31500,#31501),.UNSPECIFIED.,.F.,.F.)
B_SPLINE_CURVE_WITH_KNOTS((3,3),(0.0913980941282296,0.128154684519472),
 .UNSPECIFIED.)
CURVE()
GEOMETRIC_REPRESENTATION_ITEM()
RATIONAL_B_SPLINE_CURVE((1.00900211770901,1.00952129238837,1.00900211770901))
REPRESENTATION_ITEM('')
);
#165=(
BOUNDED_CURVE()
B_SPLINE_CURVE(2,(#31505,#31506,#31507),.UNSPECIFIED.,.F.,.F.)
B_SPLINE_CURVE_WITH_KNOTS((3,3),(0.0979198359865813,0.674024179098759),
 .UNSPECIFIED.)
CURVE()
GEOMETRIC_REPRESENTATION_ITEM()
RATIONAL_B_SPLINE_CURVE((1.0564201716687,1.19828036671056,1.0564201716687))
REPRESENTATION_ITEM('')
);
#166=(
BOUNDED_CURVE()
B_SPLINE_CURVE(2,(#31509,#31510,#31511),.UNSPECIFIED.,.F.,.F.)
B_SPLINE_CURVE_WITH_KNOTS((3,3),(0.0979198359865817,0.674024179098759),
 .UNSPECIFIED.)
CURVE()
GEOMETRIC_REPRESENTATION_ITEM()
RATIONAL_B_SPLINE_CURVE((1.0564201716687,1.19828036671056,1.0564201716687))
REPRESENTATION_ITEM('')
);
#167=(
BOUNDED_CURVE()
B_SPLINE_CURVE(2,(#31513,#31514,#31515),.UNSPECIFIED.,.F.,.F.)
B_SPLINE_CURVE_WITH_KNOTS((3,3),(0.0979198359865813,0.674024179098759),
 .UNSPECIFIED.)
CURVE()
GEOMETRIC_REPRESENTATION_ITEM()
RATIONAL_B_SPLINE_CURVE((1.0564201716687,1.19828036671056,1.0564201716687))
REPRESENTATION_ITEM('')
);
#168=(
BOUNDED_CURVE()
B_SPLINE_CURVE(2,(#31521,#31522,#31523),.UNSPECIFIED.,.F.,.F.)
B_SPLINE_CURVE_WITH_KNOTS((3,3),(0.0979198359865812,0.385972007542669),
 .UNSPECIFIED.)
CURVE()
GEOMETRIC_REPRESENTATION_ITEM()
RATIONAL_B_SPLINE_CURVE((1.0564201716687,1.12735026918963,1.12735026918963))
REPRESENTATION_ITEM('')
);
#169=(
BOUNDED_CURVE()
B_SPLINE_CURVE(2,(#31524,#31525,#31526),.UNSPECIFIED.,.F.,.F.)
B_SPLINE_CURVE_WITH_KNOTS((3,3),(0.0979198359865812,0.674024179098759),
 .UNSPECIFIED.)
CURVE()
GEOMETRIC_REPRESENTATION_ITEM()
RATIONAL_B_SPLINE_CURVE((1.0564201716687,1.19828036671056,1.0564201716687))
REPRESENTATION_ITEM('')
);
#170=(
BOUNDED_CURVE()
B_SPLINE_CURVE(2,(#31527,#31528,#31529),.UNSPECIFIED.,.F.,.F.)
B_SPLINE_CURVE_WITH_KNOTS((3,3),(0.0979198359865813,0.674024179098759),
 .UNSPECIFIED.)
CURVE()
GEOMETRIC_REPRESENTATION_ITEM()
RATIONAL_B_SPLINE_CURVE((1.0564201716687,1.19828036671056,1.0564201716687))
REPRESENTATION_ITEM('')
);
#171=(
BOUNDED_CURVE()
B_SPLINE_CURVE(2,(#31530,#31531,#31532),.UNSPECIFIED.,.F.,.F.)
B_SPLINE_CURVE_WITH_KNOTS((3,3),(0.385972007542669,0.674024179098759),
 .UNSPECIFIED.)
CURVE()
GEOMETRIC_REPRESENTATION_ITEM()
RATIONAL_B_SPLINE_CURVE((1.12735026918963,1.12735026918963,1.0564201716687))
REPRESENTATION_ITEM('')
);
#172=ELLIPSE('',#13107,0.678822509939079,0.48);
#173=ELLIPSE('',#13111,0.678822509939079,0.48);
#174=ELLIPSE('',#13114,0.678822509939079,0.48);
#175=ELLIPSE('',#13116,0.678822509939079,0.48);
#176=SPHERICAL_SURFACE('',#13012,0.23815);
#177=SPHERICAL_SURFACE('',#13037,0.23815);
#178=SPHERICAL_SURFACE('',#13043,0.23815);
#179=SPHERICAL_SURFACE('',#13050,0.23815);
#180=SPHERICAL_SURFACE('',#13056,0.23815);
#181=SPHERICAL_SURFACE('',#13062,0.23815);
#182=SPHERICAL_SURFACE('',#13073,0.23815);
#183=SHAPE_REPRESENTATION_RELATIONSHIP('SRR','None',#31705,#194);
#184=SHAPE_REPRESENTATION_RELATIONSHIP('SRR','None',#31706,#195);
#185=SHAPE_REPRESENTATION_RELATIONSHIP('SRR','None',#31707,#196);
#186=SHAPE_REPRESENTATION_RELATIONSHIP('SRR','None',#31708,#197);
#187=SHAPE_REPRESENTATION_RELATIONSHIP('SRR','None',#31709,#198);
#188=SHAPE_REPRESENTATION_RELATIONSHIP('SRR','None',#31710,#199);
#189=SHAPE_REPRESENTATION_RELATIONSHIP('SRR','None',#31711,#200);
#190=SHAPE_REPRESENTATION_RELATIONSHIP('SRR','None',#31712,#201);
#191=SHAPE_REPRESENTATION_RELATIONSHIP('SRR','None',#31713,#202);
#192=SHAPE_REPRESENTATION_RELATIONSHIP('SRR','None',#31714,#203);
#193=SHAPE_REPRESENTATION_RELATIONSHIP('SRR','None',#31715,#204);
#194=ADVANCED_BREP_SHAPE_REPRESENTATION('',(#216),#31627);
#195=ADVANCED_BREP_SHAPE_REPRESENTATION('',(#217),#31628);
#196=ADVANCED_BREP_SHAPE_REPRESENTATION('',(#218),#31629);
#197=ADVANCED_BREP_SHAPE_REPRESENTATION('',(#219),#31630);
#198=ADVANCED_BREP_SHAPE_REPRESENTATION('',(#220),#31631);
#199=ADVANCED_BREP_SHAPE_REPRESENTATION('',(#221),#31632);
#200=ADVANCED_BREP_SHAPE_REPRESENTATION('',(#222),#31633);
#201=ADVANCED_BREP_SHAPE_REPRESENTATION('',(#223),#31634);
#202=ADVANCED_BREP_SHAPE_REPRESENTATION('',(#224),#31635);
#203=ADVANCED_BREP_SHAPE_REPRESENTATION('',(#225),#31636);
#204=ADVANCED_BREP_SHAPE_REPRESENTATION('',(#226),#31637);
#205=STYLED_ITEM('',(#31809),#216);
#206=STYLED_ITEM('',(#31823),#217);
#207=STYLED_ITEM('',(#31830),#218);
#208=STYLED_ITEM('',(#31823),#219);
#209=STYLED_ITEM('',(#31830),#220);
#210=STYLED_ITEM('',(#31823),#221);
#211=STYLED_ITEM('',(#31844),#222);
#212=STYLED_ITEM('',(#31837),#223);
#213=STYLED_ITEM('',(#31837),#224);
#214=STYLED_ITEM('',(#31837),#225);
#215=STYLED_ITEM('',(#31837),#226);
#216=MANIFOLD_SOLID_BREP('Frame',#12480);
#217=MANIFOLD_SOLID_BREP('Spiral bevel gear',#12481);
#218=MANIFOLD_SOLID_BREP('Shaft',#12482);
#219=MANIFOLD_SOLID_BREP('Spiral bevel gear',#12483);
#220=MANIFOLD_SOLID_BREP('6000-ZZ rings + balls + shields',#12484);
#221=MANIFOLD_SOLID_BREP('Shim ring',#12485);
#222=MANIFOLD_SOLID_BREP('Retaining ring',#12486);
#223=MANIFOLD_SOLID_BREP('Set screw',#12487);
#224=MANIFOLD_SOLID_BREP('Socket head cap screw',#12488);
#225=MANIFOLD_SOLID_BREP('Washer',#12489);
#226=MANIFOLD_SOLID_BREP('Hex nut',#12490);
#227=TOROIDAL_SURFACE('',#12758,0.8,0.4);
#228=TOROIDAL_SURFACE('',#12761,0.8,0.4);
#229=TOROIDAL_SURFACE('',#12765,0.8,0.4);
#230=TOROIDAL_SURFACE('',#12770,0.8,0.4);
#231=TOROIDAL_SURFACE('',#13024,0.9,0.2374);
#232=TOROIDAL_SURFACE('',#13035,0.9,0.2374);
#233=TOROIDAL_SURFACE('',#13040,0.9,0.2374);
#234=TOROIDAL_SURFACE('',#13041,0.9,0.2374);
#235=TOROIDAL_SURFACE('',#13046,0.9,0.2374);
#236=TOROIDAL_SURFACE('',#13047,0.9,0.2374);
#237=TOROIDAL_SURFACE('',#13053,0.9,0.2374);
#238=TOROIDAL_SURFACE('',#13054,0.9,0.2374);
#239=TOROIDAL_SURFACE('',#13059,0.9,0.2374);
#240=TOROIDAL_SURFACE('',#13060,0.9,0.2374);
#241=TOROIDAL_SURFACE('',#13067,0.9,0.2374);
#242=TOROIDAL_SURFACE('',#13072,0.9,0.2374);
#243=TOROIDAL_SURFACE('',#13076,0.9,0.2374);
#244=TOROIDAL_SURFACE('',#13086,0.9,0.2374);
#245=TOROIDAL_SURFACE('',#13459,0.323,0.025);
#246=CYLINDRICAL_SURFACE('',#12692,0.33);
#247=CYLINDRICAL_SURFACE('',#12697,0.33);
#248=CYLINDRICAL_SURFACE('',#12702,0.33);
#249=CYLINDRICAL_SURFACE('',#12707,0.33);
#250=CYLINDRICAL_SURFACE('',#12713,1.3);
#251=CYLINDRICAL_SURFACE('',#12717,0.7);
#252=CYLINDRICAL_SURFACE('',#12721,1.3);
#253=CYLINDRICAL_SURFACE('',#12727,1.3);
#254=CYLINDRICAL_SURFACE('',#12731,0.7);
#255=CYLINDRICAL_SURFACE('',#12735,1.3);
#256=CYLINDRICAL_SURFACE('',#12740,1.3);
#257=CYLINDRICAL_SURFACE('',#12744,0.7);
#258=CYLINDRICAL_SURFACE('',#12748,1.3);
#259=CYLINDRICAL_SURFACE('',#12768,0.4);
#260=CYLINDRICAL_SURFACE('',#12772,0.4);
#261=CYLINDRICAL_SURFACE('',#12773,0.4);
#262=CYLINDRICAL_SURFACE('',#12775,0.4);
#263=CYLINDRICAL_SURFACE('',#12805,1.);
#264=CYLINDRICAL_SURFACE('',#12808,1.);
#265=CYLINDRICAL_SURFACE('',#12810,0.205);
#266=CYLINDRICAL_SURFACE('',#12811,0.205);
#267=CYLINDRICAL_SURFACE('',#12860,0.501);
#268=CYLINDRICAL_SURFACE('',#12870,0.1);
#269=CYLINDRICAL_SURFACE('',#12889,0.5);
#270=CYLINDRICAL_SURFACE('',#12893,0.48);
#271=CYLINDRICAL_SURFACE('',#12897,0.5);
#272=CYLINDRICAL_SURFACE('',#12901,1.);
#273=CYLINDRICAL_SURFACE('',#12905,1.);
#274=CYLINDRICAL_SURFACE('',#12908,0.205);
#275=CYLINDRICAL_SURFACE('',#12909,0.205);
#276=CYLINDRICAL_SURFACE('',#12981,0.501);
#277=CYLINDRICAL_SURFACE('',#12993,0.76);
#278=CYLINDRICAL_SURFACE('',#12994,1.06);
#279=CYLINDRICAL_SURFACE('',#13002,0.76);
#280=CYLINDRICAL_SURFACE('',#13003,1.06);
#281=CYLINDRICAL_SURFACE('',#13015,1.06);
#282=CYLINDRICAL_SURFACE('',#13025,0.74);
#283=CYLINDRICAL_SURFACE('',#13065,1.06);
#284=CYLINDRICAL_SURFACE('',#13068,0.74);
#285=CYLINDRICAL_SURFACE('',#13081,1.3);
#286=CYLINDRICAL_SURFACE('',#13087,0.5);
#287=CYLINDRICAL_SURFACE('',#13097,0.5);
#288=CYLINDRICAL_SURFACE('',#13102,0.8);
#289=CYLINDRICAL_SURFACE('',#13113,0.48);
#290=CYLINDRICAL_SURFACE('',#13125,0.05);
#291=CYLINDRICAL_SURFACE('',#13127,0.05);
#292=CYLINDRICAL_SURFACE('',#13135,0.6);
#293=CYLINDRICAL_SURFACE('',#13137,0.1954);
#294=CYLINDRICAL_SURFACE('',#13139,0.1954);
#295=CYLINDRICAL_SURFACE('',#13140,0.1954);
#296=CYLINDRICAL_SURFACE('',#13141,0.1954);
#297=CYLINDRICAL_SURFACE('',#13142,0.1954);
#298=CYLINDRICAL_SURFACE('',#13143,0.1954);
#299=CYLINDRICAL_SURFACE('',#13144,0.15555);
#300=CYLINDRICAL_SURFACE('',#13146,0.15555);
#301=CYLINDRICAL_SURFACE('',#13148,0.15555);
#302=CYLINDRICAL_SURFACE('',#13149,0.15555);
#303=CYLINDRICAL_SURFACE('',#13150,0.15555);
#304=CYLINDRICAL_SURFACE('',#13151,0.15555);
#305=CYLINDRICAL_SURFACE('',#13159,0.15555);
#306=CYLINDRICAL_SURFACE('',#13170,0.1954);
#307=CYLINDRICAL_SURFACE('',#13176,0.2942);
#308=CYLINDRICAL_SURFACE('',#13178,0.2942);
#309=CYLINDRICAL_SURFACE('',#13179,0.2942);
#310=CYLINDRICAL_SURFACE('',#13180,0.2942);
#311=CYLINDRICAL_SURFACE('',#13181,0.2942);
#312=CYLINDRICAL_SURFACE('',#13182,0.2942);
#313=CYLINDRICAL_SURFACE('',#13183,0.2942);
#314=CYLINDRICAL_SURFACE('',#13184,0.2942);
#315=CYLINDRICAL_SURFACE('',#13185,0.2942);
#316=CYLINDRICAL_SURFACE('',#13186,0.2942);
#317=CYLINDRICAL_SURFACE('',#13187,0.2942);
#318=CYLINDRICAL_SURFACE('',#13188,0.2942);
#319=CYLINDRICAL_SURFACE('',#13189,0.2942);
#320=CYLINDRICAL_SURFACE('',#13190,0.2942);
#321=CYLINDRICAL_SURFACE('',#13191,0.2942);
#322=CYLINDRICAL_SURFACE('',#13192,0.2942);
#323=CYLINDRICAL_SURFACE('',#13193,0.2942);
#324=CYLINDRICAL_SURFACE('',#13194,0.2942);
#325=CYLINDRICAL_SURFACE('',#13195,0.2942);
#326=CYLINDRICAL_SURFACE('',#13196,0.2942);
#327=CYLINDRICAL_SURFACE('',#13197,0.2942);
#328=CYLINDRICAL_SURFACE('',#13198,0.2942);
#329=CYLINDRICAL_SURFACE('',#13199,0.2942);
#330=CYLINDRICAL_SURFACE('',#13200,0.2942);
#331=CYLINDRICAL_SURFACE('',#13201,0.237175);
#332=CYLINDRICAL_SURFACE('',#13203,0.237175);
#333=CYLINDRICAL_SURFACE('',#13205,0.237175);
#334=CYLINDRICAL_SURFACE('',#13206,0.237175);
#335=CYLINDRICAL_SURFACE('',#13207,0.237175);
#336=CYLINDRICAL_SURFACE('',#13208,0.237175);
#337=CYLINDRICAL_SURFACE('',#13209,0.237175);
#338=CYLINDRICAL_SURFACE('',#13210,0.237175);
#339=CYLINDRICAL_SURFACE('',#13211,0.237175);
#340=CYLINDRICAL_SURFACE('',#13212,0.237175);
#341=CYLINDRICAL_SURFACE('',#13213,0.237175);
#342=CYLINDRICAL_SURFACE('',#13214,0.237175);
#343=CYLINDRICAL_SURFACE('',#13215,0.237175);
#344=CYLINDRICAL_SURFACE('',#13216,0.237175);
#345=CYLINDRICAL_SURFACE('',#13217,0.237175);
#346=CYLINDRICAL_SURFACE('',#13218,0.237175);
#347=CYLINDRICAL_SURFACE('',#13219,0.237175);
#348=CYLINDRICAL_SURFACE('',#13220,0.237175);
#349=CYLINDRICAL_SURFACE('',#13221,0.237175);
#350=CYLINDRICAL_SURFACE('',#13222,0.237175);
#351=CYLINDRICAL_SURFACE('',#13223,0.237175);
#352=CYLINDRICAL_SURFACE('',#13224,0.237175);
#353=CYLINDRICAL_SURFACE('',#13225,0.237175);
#354=CYLINDRICAL_SURFACE('',#13226,0.237175);
#355=CYLINDRICAL_SURFACE('',#13231,0.237175);
#356=CYLINDRICAL_SURFACE('',#13463,0.298);
#357=CYLINDRICAL_SURFACE('',#13470,0.2942);
#358=CYLINDRICAL_SURFACE('',#13475,0.5);
#359=CYLINDRICAL_SURFACE('',#13522,0.6);
#360=CYLINDRICAL_SURFACE('',#13528,0.32);
#361=CYLINDRICAL_SURFACE('',#13575,0.305);
#362=CONICAL_SURFACE('',#12690,0.36,0.785398163397444);
#363=CONICAL_SURFACE('',#12694,0.36,0.785398163397444);
#364=CONICAL_SURFACE('',#12695,0.36,0.785398163397444);
#365=CONICAL_SURFACE('',#12699,0.36,0.785398163397444);
#366=CONICAL_SURFACE('',#12700,0.36,0.785398163397444);
#367=CONICAL_SURFACE('',#12704,0.36,0.785398163397444);
#368=CONICAL_SURFACE('',#12705,0.36,0.785398163397444);
#369=CONICAL_SURFACE('',#12709,0.36,0.785398163397444);
#370=CONICAL_SURFACE('',#12710,1.35,0.78539816339745);
#371=CONICAL_SURFACE('',#12723,1.35,0.785398163397441);
#372=CONICAL_SURFACE('',#12725,1.35,0.785398163397451);
#373=CONICAL_SURFACE('',#12737,1.35,0.785398163397453);
#374=CONICAL_SURFACE('',#12738,1.35,0.785398163397453);
#375=CONICAL_SURFACE('',#12750,1.35,0.785398163397451);
#376=CONICAL_SURFACE('',#12777,1.39267766952966,1.17809724509617);
#377=CONICAL_SURFACE('',#12781,1.63192209588552,0.785398163397448);
#378=CONICAL_SURFACE('',#12812,0.975,0.785398163397446);
#379=CONICAL_SURFACE('',#12814,1.56260147929642,0.850360450324169);
#380=CONICAL_SURFACE('',#12816,1.56260147929642,0.850360450324169);
#381=CONICAL_SURFACE('',#12818,1.56260147929642,0.850360450324169);
#382=CONICAL_SURFACE('',#12820,1.56260147929642,0.850360450324169);
#383=CONICAL_SURFACE('',#12822,1.56260147929642,0.850360450324169);
#384=CONICAL_SURFACE('',#12824,1.56260147929642,0.850360450324169);
#385=CONICAL_SURFACE('',#12826,1.56260147929642,0.850360450324169);
#386=CONICAL_SURFACE('',#12828,1.56260147929642,0.850360450324169);
#387=CONICAL_SURFACE('',#12830,1.56260147929642,0.850360450324169);
#388=CONICAL_SURFACE('',#12832,1.56260147929642,0.850360450324169);
#389=CONICAL_SURFACE('',#12834,1.56260147929642,0.850360450324169);
#390=CONICAL_SURFACE('',#12836,1.56260147929642,0.850360450324169);
#391=CONICAL_SURFACE('',#12838,1.56260147929642,0.850360450324169);
#392=CONICAL_SURFACE('',#12840,1.56260147929642,0.850360450324169);
#393=CONICAL_SURFACE('',#12842,1.56260147929642,0.850360450324169);
#394=CONICAL_SURFACE('',#12844,1.56260147929642,0.850360450324169);
#395=CONICAL_SURFACE('',#12846,1.56260147929642,0.850360450324169);
#396=CONICAL_SURFACE('',#12848,1.56260147929642,0.850360450324169);
#397=CONICAL_SURFACE('',#12850,1.56260147929642,0.850360450324169);
#398=CONICAL_SURFACE('',#12852,0.980679383410898,0.785398163397448);
#399=CONICAL_SURFACE('',#12855,1.56260147929642,0.850360450324169);
#400=CONICAL_SURFACE('',#12858,0.521,0.785398163397448);
#401=CONICAL_SURFACE('',#12862,0.521,0.785398163397451);
#402=CONICAL_SURFACE('',#12866,0.12,0.785398163397459);
#403=CONICAL_SURFACE('',#12874,0.05,1.03037682652432);
#404=CONICAL_SURFACE('',#12887,0.475,0.785398163397448);
#405=CONICAL_SURFACE('',#12899,0.475,0.785398163397441);
#406=CONICAL_SURFACE('',#12910,0.975,0.785398163397446);
#407=CONICAL_SURFACE('',#12912,1.63192209588552,0.785398163397448);
#408=CONICAL_SURFACE('',#12934,1.56260147929642,0.850360450324169);
#409=CONICAL_SURFACE('',#12936,1.56260147929642,0.850360450324169);
#410=CONICAL_SURFACE('',#12938,1.56260147929642,0.850360450324169);
#411=CONICAL_SURFACE('',#12940,1.56260147929642,0.850360450324169);
#412=CONICAL_SURFACE('',#12942,1.56260147929642,0.850360450324169);
#413=CONICAL_SURFACE('',#12944,1.56260147929642,0.850360450324169);
#414=CONICAL_SURFACE('',#12946,1.56260147929642,0.850360450324169);
#415=CONICAL_SURFACE('',#12948,1.56260147929642,0.850360450324169);
#416=CONICAL_SURFACE('',#12950,1.56260147929642,0.850360450324169);
#417=CONICAL_SURFACE('',#12952,1.56260147929642,0.850360450324169);
#418=CONICAL_SURFACE('',#12954,1.56260147929642,0.850360450324169);
#419=CONICAL_SURFACE('',#12956,1.56260147929642,0.850360450324169);
#420=CONICAL_SURFACE('',#12958,1.56260147929642,0.850360450324169);
#421=CONICAL_SURFACE('',#12960,1.56260147929642,0.850360450324169);
#422=CONICAL_SURFACE('',#12962,1.56260147929642,0.850360450324169);
#423=CONICAL_SURFACE('',#12964,1.56260147929642,0.850360450324169);
#424=CONICAL_SURFACE('',#12966,1.56260147929642,0.850360450324169);
#425=CONICAL_SURFACE('',#12968,1.56260147929642,0.850360450324169);
#426=CONICAL_SURFACE('',#12970,1.56260147929642,0.850360450324169);
#427=CONICAL_SURFACE('',#12972,0.980679383410898,0.785398163397448);
#428=CONICAL_SURFACE('',#12975,1.56260147929642,0.850360450324169);
#429=CONICAL_SURFACE('',#12979,0.521,0.785398163397448);
#430=CONICAL_SURFACE('',#12983,0.521,0.785398163397451);
#431=CONICAL_SURFACE('',#13079,1.285,0.785398163397452);
#432=CONICAL_SURFACE('',#13083,1.285,0.785398163397452);
#433=CONICAL_SURFACE('',#13090,0.515,0.785398163397452);
#434=CONICAL_SURFACE('',#13095,0.515,0.785398163397452);
#435=CONICAL_SURFACE('',#13169,0.185,0.785398163397445);
#436=CONICAL_SURFACE('',#13172,0.1625,0.785398163397447);
#437=CONICAL_SURFACE('',#13232,0.124996333279554,1.03037682652431);
#438=CONICAL_SURFACE('',#13469,0.28,0.785398163397448);
#439=CONICAL_SURFACE('',#13473,0.49,0.785398163397449);
#440=CONICAL_SURFACE('',#13512,0.48,0.785398163397448);
#441=CONICAL_SURFACE('',#13516,0.59,0.785398163397449);
#442=CONICAL_SURFACE('',#13524,0.33,0.785398163397449);
#443=CONICAL_SURFACE('',#13533,0.33,0.785398163397449);
#444=CONICAL_SURFACE('',#13534,0.59,0.785398163397449);
#445=CONICAL_SURFACE('',#13551,0.551175134594813,1.0471975511966);
#446=CONICAL_SURFACE('',#13553,0.551175134594813,1.0471975511966);
#447=CONICAL_SURFACE('',#13555,0.551175134594813,1.0471975511966);
#448=CONICAL_SURFACE('',#13557,0.551175134594813,1.0471975511966);
#449=CONICAL_SURFACE('',#13559,0.551175134594813,1.0471975511966);
#450=CONICAL_SURFACE('',#13561,0.551175134594813,1.0471975511966);
#451=CONICAL_SURFACE('',#13563,0.551175134594813,1.0471975511966);
#452=CONICAL_SURFACE('',#13565,0.473593266739736,1.30899693899575);
#453=CONICAL_SURFACE('',#13569,0.348075378797541,1.17809724509617);
#454=CONICAL_SURFACE('',#13571,0.325,0.785398163397448);
#455=CONICAL_SURFACE('',#13573,0.312424621202459,0.392699081698723);
#456=CONICAL_SURFACE('',#13577,0.325,0.785398163397448);
#457=B_SPLINE_CURVE_WITH_KNOTS('',3,(#16701,#16702,#16703,#16704),
 .UNSPECIFIED.,.F.,.F.,(4,4),(0.,1.),.UNSPECIFIED.);
#458=B_SPLINE_CURVE_WITH_KNOTS('',3,(#16705,#16706,#16707,#16708),
 .UNSPECIFIED.,.F.,.F.,(4,4),(-5.39792313687514,-5.36678788880707),
 .UNSPECIFIED.);
#459=B_SPLINE_CURVE_WITH_KNOTS('',3,(#16709,#16710,#16711,#16712),
 .UNSPECIFIED.,.F.,.F.,(4,4),(5.36678788880707,5.39792313687514),
 .UNSPECIFIED.);
#460=B_SPLINE_CURVE_WITH_KNOTS('',3,(#16730,#16731,#16732,#16733),
 .UNSPECIFIED.,.F.,.F.,(4,4),(0.,1.),.UNSPECIFIED.);
#461=B_SPLINE_CURVE_WITH_KNOTS('',3,(#16734,#16735,#16736,#16737),
 .UNSPECIFIED.,.F.,.F.,(4,4),(-1.,0.),.UNSPECIFIED.);
#462=B_SPLINE_CURVE_WITH_KNOTS('',3,(#16740,#16741,#16742,#16743,#16744,
#16745,#16746,#16747,#16748),.UNSPECIFIED.,.F.,.F.,(4,1,1,1,1,1,4),(0.0919588831913347,
0.287428968788757,0.385164011587469,0.48289905438618,0.580634097184891,
0.678369139983603,0.776104182782314),.UNSPECIFIED.);
#463=B_SPLINE_CURVE_WITH_KNOTS('',3,(#16750,#16751,#16752,#16753),
 .UNSPECIFIED.,.F.,.F.,(4,4),(-1.,0.),.UNSPECIFIED.);
#464=B_SPLINE_CURVE_WITH_KNOTS('',3,(#16757,#16758,#16759,#16760),
 .UNSPECIFIED.,.F.,.F.,(4,4),(0.,1.),.UNSPECIFIED.);
#465=B_SPLINE_CURVE_WITH_KNOTS('',3,(#16762,#16763,#16764,#16765,#16766,
#16767,#16768,#16769,#16770),.UNSPECIFIED.,.F.,.F.,(4,1,1,1,2,4),(2.02212896015404,
2.13032466905734,2.23852037796064,2.34671608686394,2.56310750467053,2.7062742594363),
 .UNSPECIFIED.);
#466=B_SPLINE_CURVE_WITH_KNOTS('',3,(#16772,#16773,#16774,#16775),
 .UNSPECIFIED.,.F.,.F.,(4,4),(0.,1.),.UNSPECIFIED.);
#467=B_SPLINE_CURVE_WITH_KNOTS('',3,(#16777,#16778,#16779,#16780),
 .UNSPECIFIED.,.F.,.F.,(4,4),(-0.333212111192934,-0.302076863348255),
 .UNSPECIFIED.);
#468=B_SPLINE_CURVE_WITH_KNOTS('',3,(#16816,#16817,#16818,#16819),
 .UNSPECIFIED.,.F.,.F.,(4,4),(5.36678788880707,5.40717967697245),
 .UNSPECIFIED.);
#469=B_SPLINE_CURVE_WITH_KNOTS('',3,(#16848,#16849,#16850,#16851),
 .UNSPECIFIED.,.F.,.F.,(4,4),(-1.,0.),.UNSPECIFIED.);
#470=B_SPLINE_CURVE_WITH_KNOTS('',3,(#16852,#16853,#16854,#16855),
 .UNSPECIFIED.,.F.,.F.,(4,4),(0.302076863348255,0.333212111192934),
 .UNSPECIFIED.);
#471=B_SPLINE_CURVE_WITH_KNOTS('',3,(#16872,#16873,#16874,#16875),
 .UNSPECIFIED.,.F.,.F.,(4,4),(-1.,0.),.UNSPECIFIED.);
#472=B_SPLINE_CURVE_WITH_KNOTS('',3,(#16906,#16907,#16908,#16909),
 .UNSPECIFIED.,.F.,.F.,(4,4),(0.,1.),.UNSPECIFIED.);
#473=B_SPLINE_CURVE_WITH_KNOTS('',3,(#16910,#16911,#16912,#16913),
 .UNSPECIFIED.,.F.,.F.,(4,4),(0.302076863124856,0.333212111192934),
 .UNSPECIFIED.);
#474=B_SPLINE_CURVE_WITH_KNOTS('',3,(#16914,#16915,#16916,#16917),
 .UNSPECIFIED.,.F.,.F.,(4,4),(-0.333212111192934,-0.302076863124856),
 .UNSPECIFIED.);
#475=B_SPLINE_CURVE_WITH_KNOTS('',3,(#16935,#16936,#16937,#16938),
 .UNSPECIFIED.,.F.,.F.,(4,4),(0.,1.),.UNSPECIFIED.);
#476=B_SPLINE_CURVE_WITH_KNOTS('',3,(#16939,#16940,#16941,#16942),
 .UNSPECIFIED.,.F.,.F.,(4,4),(-1.,0.),.UNSPECIFIED.);
#477=B_SPLINE_CURVE_WITH_KNOTS('',3,(#16945,#16946,#16947,#16948,#16949,
#16950,#16951,#16952),.UNSPECIFIED.,.F.,.F.,(4,1,1,1,1,4),(0.091958883192206,
0.287428968789379,0.482899054386553,0.531766575785846,0.678369139983726,
0.776104182782313),.UNSPECIFIED.);
#478=B_SPLINE_CURVE_WITH_KNOTS('',3,(#16954,#16955,#16956,#16957),
 .UNSPECIFIED.,.F.,.F.,(4,4),(-1.,0.),.UNSPECIFIED.);
#479=B_SPLINE_CURVE_WITH_KNOTS('',3,(#16961,#16962,#16963,#16964),
 .UNSPECIFIED.,.F.,.F.,(4,4),(0.,1.),.UNSPECIFIED.);
#480=B_SPLINE_CURVE_WITH_KNOTS('',3,(#16966,#16967,#16968,#16969,#16970,
#16971,#16972,#16973,#16974),.UNSPECIFIED.,.F.,.F.,(4,1,1,1,2,4),(2.02212896015404,
2.13032466905734,2.23852037796064,2.34671608686394,2.56310750467053,2.70627425943714),
 .UNSPECIFIED.);
#481=B_SPLINE_CURVE_WITH_KNOTS('',3,(#16976,#16977,#16978,#16979),
 .UNSPECIFIED.,.F.,.F.,(4,4),(0.,1.),.UNSPECIFIED.);
#482=B_SPLINE_CURVE_WITH_KNOTS('',3,(#16981,#16982,#16983,#16984),
 .UNSPECIFIED.,.F.,.F.,(4,4),(5.36678788880707,5.39792313665175),
 .UNSPECIFIED.);
#483=B_SPLINE_CURVE_WITH_KNOTS('',3,(#17020,#17021,#17022,#17023),
 .UNSPECIFIED.,.F.,.F.,(4,4),(-0.333212111192934,-0.292820323027551),
 .UNSPECIFIED.);
#484=B_SPLINE_CURVE_WITH_KNOTS('',3,(#17057,#17058,#17059,#17060),
 .UNSPECIFIED.,.F.,.F.,(4,4),(-1.,0.),.UNSPECIFIED.);
#485=B_SPLINE_CURVE_WITH_KNOTS('',3,(#17061,#17062,#17063,#17064),
 .UNSPECIFIED.,.F.,.F.,(4,4),(-5.39792313665175,-5.36678788880707),
 .UNSPECIFIED.);
#486=B_SPLINE_CURVE_WITH_KNOTS('',3,(#17081,#17082,#17083,#17084),
 .UNSPECIFIED.,.F.,.F.,(4,4),(-1.,0.),.UNSPECIFIED.);
#487=B_SPLINE_CURVE_WITH_KNOTS('',3,(#17238,#17239,#17240,#17241),
 .UNSPECIFIED.,.F.,.F.,(4,4),(0.,1.),.UNSPECIFIED.);
#488=B_SPLINE_CURVE_WITH_KNOTS('',3,(#17242,#17243,#17244,#17245,#17246,
#17247,#17248,#17249,#17250),.UNSPECIFIED.,.F.,.F.,(4,1,1,1,1,1,4),(-0.776104182782314,
-0.678369139983603,-0.580634097184891,-0.48289905438618,-0.385164011587469,
-0.287428968788757,-0.0919588831913347),.UNSPECIFIED.);
#489=B_SPLINE_CURVE_WITH_KNOTS('',3,(#17284,#17285,#17286,#17287),
 .UNSPECIFIED.,.F.,.F.,(4,4),(0.,1.),.UNSPECIFIED.);
#490=B_SPLINE_CURVE_WITH_KNOTS('',3,(#17288,#17289,#17290,#17291,#17292,
#17293,#17294,#17295),.UNSPECIFIED.,.F.,.F.,(4,1,1,1,1,4),(-0.776104182782313,
-0.678369139983726,-0.531766575785846,-0.482899054386553,-0.287428968789379,
-0.091958883192206),.UNSPECIFIED.);
#491=B_SPLINE_CURVE_WITH_KNOTS('',3,(#17340,#17341,#17342,#17343),
 .UNSPECIFIED.,.F.,.F.,(4,4),(-1.,0.),.UNSPECIFIED.);
#492=B_SPLINE_CURVE_WITH_KNOTS('',3,(#17345,#17346,#17347,#17348,#17349,
#17350,#17351,#17352,#17353),.UNSPECIFIED.,.F.,.F.,(4,2,1,1,1,4),(-2.7062742594363,
-2.56310750467053,-2.34671608686394,-2.23852037796064,-2.13032466905734,
-2.02212896015404),.UNSPECIFIED.);
#493=B_SPLINE_CURVE_WITH_KNOTS('',3,(#17371,#17372,#17373,#17374),
 .UNSPECIFIED.,.F.,.F.,(4,4),(0.292820323027551,0.333212111192934),
 .UNSPECIFIED.);
#494=B_SPLINE_CURVE_WITH_KNOTS('',3,(#17412,#17413,#17414,#17415),
 .UNSPECIFIED.,.F.,.F.,(4,4),(-1.,0.),.UNSPECIFIED.);
#495=B_SPLINE_CURVE_WITH_KNOTS('',3,(#17417,#17418,#17419,#17420,#17421,
#17422,#17423,#17424,#17425),.UNSPECIFIED.,.F.,.F.,(4,2,1,1,1,4),(-2.70627425943714,
-2.56310750467053,-2.34671608686394,-2.23852037796064,-2.13032466905734,
-2.02212896015404),.UNSPECIFIED.);
#496=B_SPLINE_CURVE_WITH_KNOTS('',3,(#17443,#17444,#17445,#17446),
 .UNSPECIFIED.,.F.,.F.,(4,4),(-5.40717967697245,-5.36678788880707),
 .UNSPECIFIED.);
#497=B_SPLINE_CURVE_WITH_KNOTS('',3,(#17463,#17464,#17465,#17466),
 .UNSPECIFIED.,.F.,.F.,(4,4),(0.,1.),.UNSPECIFIED.);
#498=B_SPLINE_CURVE_WITH_KNOTS('',3,(#17483,#17484,#17485,#17486),
 .UNSPECIFIED.,.F.,.F.,(4,4),(0.,1.),.UNSPECIFIED.);
#499=B_SPLINE_CURVE_WITH_KNOTS('',3,(#17503,#17504,#17505,#17506),
 .UNSPECIFIED.,.F.,.F.,(4,4),(-1.,0.),.UNSPECIFIED.);
#500=B_SPLINE_CURVE_WITH_KNOTS('',3,(#17523,#17524,#17525,#17526),
 .UNSPECIFIED.,.F.,.F.,(4,4),(-1.,0.),.UNSPECIFIED.);
#501=B_SPLINE_CURVE_WITH_KNOTS('',3,(#17566,#17567,#17568,#17569,#17570,
#17571,#17572,#17573),.UNSPECIFIED.,.F.,.F.,(4,2,2,4),(0.149692773523897,
0.272438948836772,0.38754999579811,0.470116529869204),.UNSPECIFIED.);
#502=B_SPLINE_CURVE_WITH_KNOTS('',3,(#17575,#17576,#17577,#17578,#17579,
#17580,#17581),.UNSPECIFIED.,.F.,.F.,(4,3,4),(0.,0.0936389480740432,0.191756090575866),
 .UNSPECIFIED.);
#503=B_SPLINE_CURVE_WITH_KNOTS('',3,(#17583,#17584,#17585,#17586,#17587,
#17588),.UNSPECIFIED.,.F.,.F.,(4,2,4),(0.,0.200149552465016,0.391670798584888),
 .UNSPECIFIED.);
#504=B_SPLINE_CURVE_WITH_KNOTS('',3,(#17592,#17593,#17594,#17595,#17596,
#17597,#17598,#17599),.UNSPECIFIED.,.F.,.F.,(4,2,2,4),(0.0766926694683487,
0.272438948824957,0.387549995788498,0.470116529871579),.UNSPECIFIED.);
#505=B_SPLINE_CURVE_WITH_KNOTS('',3,(#17601,#17602,#17603,#17604,#17605,
#17606,#17607),.UNSPECIFIED.,.F.,.F.,(4,3,4),(0.,0.0936389480740869,0.191756090576058),
 .UNSPECIFIED.);
#506=B_SPLINE_CURVE_WITH_KNOTS('',3,(#17609,#17610,#17611,#17612,#17613,
#17614),.UNSPECIFIED.,.F.,.F.,(4,2,4),(0.,0.200149552461942,0.391670798543005),
 .UNSPECIFIED.);
#507=B_SPLINE_CURVE_WITH_KNOTS('',3,(#17618,#17619,#17620,#17621,#17622,
#17623,#17624,#17625),.UNSPECIFIED.,.F.,.F.,(4,2,2,4),(0.07669266946791,
0.272438948814009,0.387549995787584,0.470116529878316),.UNSPECIFIED.);
#508=B_SPLINE_CURVE_WITH_KNOTS('',3,(#17627,#17628,#17629,#17630,#17631,
#17632,#17633),.UNSPECIFIED.,.F.,.F.,(4,3,4),(0.,0.093638948074052,0.191756090575907),
 .UNSPECIFIED.);
#509=B_SPLINE_CURVE_WITH_KNOTS('',3,(#17635,#17636,#17637,#17638,#17639,
#17640),.UNSPECIFIED.,.F.,.F.,(4,2,4),(0.,0.200149552452443,0.391670798540186),
 .UNSPECIFIED.);
#510=B_SPLINE_CURVE_WITH_KNOTS('',3,(#17644,#17645,#17646,#17647,#17648,
#17649,#17650,#17651),.UNSPECIFIED.,.F.,.F.,(4,2,2,4),(0.0766926694699025,
0.27243894883796,0.387549995810096,0.470116529899442),.UNSPECIFIED.);
#511=B_SPLINE_CURVE_WITH_KNOTS('',3,(#17653,#17654,#17655,#17656,#17657,
#17658,#17659),.UNSPECIFIED.,.F.,.F.,(4,3,4),(0.,0.0936389480740974,0.191756090576102),
 .UNSPECIFIED.);
#512=B_SPLINE_CURVE_WITH_KNOTS('',3,(#17661,#17662,#17663,#17664,#17665,
#17666),.UNSPECIFIED.,.F.,.F.,(4,2,4),(0.,0.200149552471508,0.391670798610117),
 .UNSPECIFIED.);
#513=B_SPLINE_CURVE_WITH_KNOTS('',3,(#17670,#17671,#17672,#17673,#17674,
#17675,#17676,#17677),.UNSPECIFIED.,.F.,.F.,(4,2,2,4),(0.0766926694689824,
0.272438948828123,0.387549995794212,0.47011652987127),.UNSPECIFIED.);
#514=B_SPLINE_CURVE_WITH_KNOTS('',3,(#17679,#17680,#17681,#17682,#17683,
#17684,#17685),.UNSPECIFIED.,.F.,.F.,(4,3,4),(0.,0.0936389480740665,0.191756090575991),
 .UNSPECIFIED.);
#515=B_SPLINE_CURVE_WITH_KNOTS('',3,(#17687,#17688,#17689,#17690,#17691,
#17692),.UNSPECIFIED.,.F.,.F.,(4,2,4),(0.,0.200149552469487,0.327652992715533),
 .UNSPECIFIED.);
#516=B_SPLINE_CURVE_WITH_KNOTS('',3,(#17696,#17697,#17698,#17699,#17700,
#17701,#17702,#17703),.UNSPECIFIED.,.F.,.F.,(4,2,2,4),(0.0766926694695153,
0.272438948836664,0.387549995798075,0.47011652986564),.UNSPECIFIED.);
#517=B_SPLINE_CURVE_WITH_KNOTS('',3,(#17705,#17706,#17707,#17708,#17709,
#17710,#17711),.UNSPECIFIED.,.F.,.F.,(4,3,4),(0.,0.0936389480740678,0.191756090575965),
 .UNSPECIFIED.);
#518=B_SPLINE_CURVE_WITH_KNOTS('',3,(#17713,#17714,#17715,#17716,#17717,
#17718),.UNSPECIFIED.,.F.,.F.,(4,2,4),(0.,0.200149552470465,0.391670798620175),
 .UNSPECIFIED.);
#519=B_SPLINE_CURVE_WITH_KNOTS('',3,(#17722,#17723,#17724,#17725,#17726,
#17727,#17728,#17729),.UNSPECIFIED.,.F.,.F.,(4,2,2,4),(0.0766926694689144,
0.272438948826603,0.387549995797168,0.47011652988698),.UNSPECIFIED.);
#520=B_SPLINE_CURVE_WITH_KNOTS('',3,(#17731,#17732,#17733,#17734,#17735,
#17736,#17737),.UNSPECIFIED.,.F.,.F.,(4,3,4),(0.,0.0936389480740579,0.191756090575915),
 .UNSPECIFIED.);
#521=B_SPLINE_CURVE_WITH_KNOTS('',3,(#17739,#17740,#17741,#17742,#17743,
#17744),.UNSPECIFIED.,.F.,.F.,(4,2,4),(0.,0.200149552468106,0.391670798588367),
 .UNSPECIFIED.);
#522=B_SPLINE_CURVE_WITH_KNOTS('',3,(#17748,#17749,#17750,#17751,#17752,
#17753,#17754,#17755),.UNSPECIFIED.,.F.,.F.,(4,2,2,4),(0.0766926694722585,
0.272438948867033,0.387549995827054,0.470116529890559),.UNSPECIFIED.);
#523=B_SPLINE_CURVE_WITH_KNOTS('',3,(#17757,#17758,#17759,#17760,#17761,
#17762,#17763),.UNSPECIFIED.,.F.,.F.,(4,3,4),(0.,0.0936389480740453,0.191756090575874),
 .UNSPECIFIED.);
#524=B_SPLINE_CURVE_WITH_KNOTS('',3,(#17765,#17766,#17767,#17768,#17769,
#17770),.UNSPECIFIED.,.F.,.F.,(4,2,4),(0.,0.200149552459509,0.391670798578034),
 .UNSPECIFIED.);
#525=B_SPLINE_CURVE_WITH_KNOTS('',3,(#17774,#17775,#17776,#17777,#17778,
#17779,#17780,#17781),.UNSPECIFIED.,.F.,.F.,(4,2,2,4),(0.0766926694700454,
0.272438948841727,0.387549995804977,0.470116529879896),.UNSPECIFIED.);
#526=B_SPLINE_CURVE_WITH_KNOTS('',3,(#17783,#17784,#17785,#17786,#17787,
#17788,#17789),.UNSPECIFIED.,.F.,.F.,(4,3,4),(0.,0.0936389480740846,0.191756090576072),
 .UNSPECIFIED.);
#527=B_SPLINE_CURVE_WITH_KNOTS('',3,(#17791,#17792,#17793,#17794,#17795,
#17796),.UNSPECIFIED.,.F.,.F.,(4,2,4),(0.,0.200149552458071,0.391670798531918),
 .UNSPECIFIED.);
#528=B_SPLINE_CURVE_WITH_KNOTS('',3,(#17800,#17801,#17802,#17803,#17804,
#17805,#17806,#17807),.UNSPECIFIED.,.F.,.F.,(4,2,2,4),(0.0766926694689764,
0.272438948828007,0.387549995794164,0.470116529870617),.UNSPECIFIED.);
#529=B_SPLINE_CURVE_WITH_KNOTS('',3,(#17809,#17810,#17811,#17812,#17813,
#17814,#17815),.UNSPECIFIED.,.F.,.F.,(4,3,4),(0.,0.0936389480741051,0.191756090576146),
 .UNSPECIFIED.);
#530=B_SPLINE_CURVE_WITH_KNOTS('',3,(#17817,#17818,#17819,#17820,#17821,
#17822),.UNSPECIFIED.,.F.,.F.,(4,2,4),(0.,0.200149552457873,0.327652992693914),
 .UNSPECIFIED.);
#531=B_SPLINE_CURVE_WITH_KNOTS('',3,(#17826,#17827,#17828,#17829,#17830,
#17831,#17832,#17833),.UNSPECIFIED.,.F.,.F.,(4,2,2,4),(0.0766926694699692,
0.272438948839556,0.387549995809595,0.470116529895468),.UNSPECIFIED.);
#532=B_SPLINE_CURVE_WITH_KNOTS('',3,(#17835,#17836,#17837,#17838,#17839,
#17840,#17841),.UNSPECIFIED.,.F.,.F.,(4,3,4),(0.,0.0936389480740616,0.191756090575948),
 .UNSPECIFIED.);
#533=B_SPLINE_CURVE_WITH_KNOTS('',3,(#17843,#17844,#17845,#17846,#17847,
#17848),.UNSPECIFIED.,.F.,.F.,(4,2,4),(0.,0.200149552455358,0.391670798525636),
 .UNSPECIFIED.);
#534=B_SPLINE_CURVE_WITH_KNOTS('',3,(#17852,#17853,#17854,#17855,#17856,
#17857,#17858,#17859),.UNSPECIFIED.,.F.,.F.,(4,2,2,4),(0.0766926694698568,
0.272438948838172,0.387549995805395,0.470116529884337),.UNSPECIFIED.);
#535=B_SPLINE_CURVE_WITH_KNOTS('',3,(#17861,#17862,#17863,#17864,#17865,
#17866,#17867),.UNSPECIFIED.,.F.,.F.,(4,3,4),(0.,0.0936389480740228,0.191756090575811),
 .UNSPECIFIED.);
#536=B_SPLINE_CURVE_WITH_KNOTS('',3,(#17869,#17870,#17871,#17872,#17873,
#17874),.UNSPECIFIED.,.F.,.F.,(4,2,4),(0.,0.200149552470612,0.391670798618823),
 .UNSPECIFIED.);
#537=B_SPLINE_CURVE_WITH_KNOTS('',3,(#17878,#17879,#17880,#17881,#17882,
#17883,#17884,#17885),.UNSPECIFIED.,.F.,.F.,(4,2,2,4),(0.0766926694692372,
0.272438948831663,0.387549995799224,0.470116529873121),.UNSPECIFIED.);
#538=B_SPLINE_CURVE_WITH_KNOTS('',3,(#17887,#17888,#17889,#17890,#17891,
#17892,#17893),.UNSPECIFIED.,.F.,.F.,(4,3,4),(0.,0.0936389480740782,0.19175609057602),
 .UNSPECIFIED.);
#539=B_SPLINE_CURVE_WITH_KNOTS('',3,(#17895,#17896,#17897,#17898,#17899,
#17900),.UNSPECIFIED.,.F.,.F.,(4,2,4),(0.,0.200149552459575,0.391670798562508),
 .UNSPECIFIED.);
#540=B_SPLINE_CURVE_WITH_KNOTS('',3,(#17904,#17905,#17906,#17907,#17908,
#17909,#17910,#17911),.UNSPECIFIED.,.F.,.F.,(4,2,2,4),(0.0766926694691861,
0.272438948833637,0.387549995804666,0.470116529896578),.UNSPECIFIED.);
#541=B_SPLINE_CURVE_WITH_KNOTS('',3,(#17913,#17914,#17915,#17916,#17917,
#17918,#17919),.UNSPECIFIED.,.F.,.F.,(4,3,4),(0.,0.093638948074071,0.191756090576001),
 .UNSPECIFIED.);
#542=B_SPLINE_CURVE_WITH_KNOTS('',3,(#17921,#17922,#17923,#17924,#17925,
#17926),.UNSPECIFIED.,.F.,.F.,(4,2,4),(0.,0.20014955246592,0.39167079859368),
 .UNSPECIFIED.);
#543=B_SPLINE_CURVE_WITH_KNOTS('',3,(#17930,#17931,#17932,#17933,#17934,
#17935,#17936,#17937),.UNSPECIFIED.,.F.,.F.,(4,2,2,4),(0.0766926694700761,
0.27243894884306,0.387549995806336,0.470116529880931),.UNSPECIFIED.);
#544=B_SPLINE_CURVE_WITH_KNOTS('',3,(#17939,#17940,#17941,#17942,#17943,
#17944,#17945),.UNSPECIFIED.,.F.,.F.,(4,3,4),(0.,0.0936389480740579,0.191756090575929),
 .UNSPECIFIED.);
#545=B_SPLINE_CURVE_WITH_KNOTS('',3,(#17947,#17948,#17949,#17950,#17951,
#17952),.UNSPECIFIED.,.F.,.F.,(4,2,4),(0.,0.200149552465185,0.327652992740583),
 .UNSPECIFIED.);
#546=B_SPLINE_CURVE_WITH_KNOTS('',3,(#17956,#17957,#17958,#17959,#17960,
#17961,#17962,#17963),.UNSPECIFIED.,.F.,.F.,(4,2,2,4),(0.0766926694694027,
0.272438948835416,0.38754999579658,0.470116529865663),.UNSPECIFIED.);
#547=B_SPLINE_CURVE_WITH_KNOTS('',3,(#17965,#17966,#17967,#17968,#17969,
#17970,#17971),.UNSPECIFIED.,.F.,.F.,(4,3,4),(0.,0.0936389480740775,0.191756090576017),
 .UNSPECIFIED.);
#548=B_SPLINE_CURVE_WITH_KNOTS('',3,(#17973,#17974,#17975,#17976,#17977,
#17978),.UNSPECIFIED.,.F.,.F.,(4,2,4),(0.,0.200149552466382,0.391670798591391),
 .UNSPECIFIED.);
#549=B_SPLINE_CURVE_WITH_KNOTS('',3,(#17982,#17983,#17984,#17985,#17986,
#17987,#17988,#17989),.UNSPECIFIED.,.F.,.F.,(4,2,2,4),(0.0766926694683472,
0.272438948824933,0.387549995788448,0.470116529871442),.UNSPECIFIED.);
#550=B_SPLINE_CURVE_WITH_KNOTS('',3,(#17991,#17992,#17993,#17994,#17995,
#17996,#17997),.UNSPECIFIED.,.F.,.F.,(4,3,4),(0.,0.0936389480740692,0.19175609057597),
 .UNSPECIFIED.);
#551=B_SPLINE_CURVE_WITH_KNOTS('',3,(#17999,#18000,#18001,#18002,#18003,
#18004),.UNSPECIFIED.,.F.,.F.,(4,2,4),(0.,0.200149552469509,0.391670798593535),
 .UNSPECIFIED.);
#552=B_SPLINE_CURVE_WITH_KNOTS('',3,(#18008,#18009,#18010,#18011,#18012,
#18013,#18014,#18015),.UNSPECIFIED.,.F.,.F.,(4,2,2,4),(0.0766926694679092,
0.272438948814003,0.387549995787569,0.470116529878258),.UNSPECIFIED.);
#553=B_SPLINE_CURVE_WITH_KNOTS('',3,(#18017,#18018,#18019,#18020,#18021,
#18022,#18023),.UNSPECIFIED.,.F.,.F.,(4,3,4),(0.,0.093638948074058,0.191756090575958),
 .UNSPECIFIED.);
#554=B_SPLINE_CURVE_WITH_KNOTS('',3,(#18025,#18026,#18027,#18028,#18029,
#18030),.UNSPECIFIED.,.F.,.F.,(4,2,4),(0.,0.200149552458024,0.391670798575916),
 .UNSPECIFIED.);
#555=B_SPLINE_CURVE_WITH_KNOTS('',3,(#18034,#18035,#18036,#18037,#18038,
#18039,#18040,#18041),.UNSPECIFIED.,.F.,.F.,(4,2,2,4),(0.076692669469278,
0.272438948829378,0.387549995792969,0.47011652986107),.UNSPECIFIED.);
#556=B_SPLINE_CURVE_WITH_KNOTS('',3,(#18043,#18044,#18045,#18046,#18047,
#18048,#18049),.UNSPECIFIED.,.F.,.F.,(4,3,4),(0.,0.093638948074072,0.191756090575973),
 .UNSPECIFIED.);
#557=B_SPLINE_CURVE_WITH_KNOTS('',3,(#18051,#18052,#18053,#18054,#18055,
#18056),.UNSPECIFIED.,.F.,.F.,(4,2,4),(0.,0.200149552458622,0.391670798526984),
 .UNSPECIFIED.);
#558=B_SPLINE_CURVE_WITH_KNOTS('',3,(#18060,#18061,#18062,#18063,#18064,
#18065,#18066,#18067),.UNSPECIFIED.,.F.,.F.,(4,2,2,4),(0.0766926694689178,
0.272438948827195,0.387549995791794,0.470116529864375),.UNSPECIFIED.);
#559=B_SPLINE_CURVE_WITH_KNOTS('',3,(#18069,#18070,#18071,#18072,#18073,
#18074,#18075),.UNSPECIFIED.,.F.,.F.,(4,3,4),(0.,0.0936389480740925,0.191756090576061),
 .UNSPECIFIED.);
#560=B_SPLINE_CURVE_WITH_KNOTS('',3,(#18077,#18078,#18079,#18080,#18081,
#18082),.UNSPECIFIED.,.F.,.F.,(4,2,4),(0.,0.200149552462937,0.327652992716261),
 .UNSPECIFIED.);
#561=B_SPLINE_CURVE_WITH_KNOTS('',3,(#18085,#18086,#18087,#18088),
 .UNSPECIFIED.,.F.,.F.,(4,4),(0.076692669469509,0.149692773523897),
 .UNSPECIFIED.);
#562=B_SPLINE_CURVE_WITH_KNOTS('',3,(#18094,#18095,#18096,#18097,#18098,
#18099,#18100,#18101,#18102,#18103,#18104,#18105,#18106,#18107,#18108,#18109,
#18110,#18111,#18112,#18113,#18114,#18115,#18116,#18117,#18118,#18119,#18120,
#18121,#18122,#18123,#18124,#18125,#18126,#18127,#18128,#18129,#18130),
 .UNSPECIFIED.,.F.,.F.,(4,3,3,3,3,3,3,3,3,3,3,3,4),(0.,0.0140126898858465,
0.0198365927950119,0.0393688637311589,0.0455583406050571,0.0493231568139791,
0.0527005792494364,0.0569161964938546,0.0651768568751002,0.0683276956644967,
0.0828398890011837,0.0964479725722503,0.100882854087323),.UNSPECIFIED.);
#563=B_SPLINE_CURVE_WITH_KNOTS('',3,(#18133,#18134,#18135,#18136,#18137,
#18138,#18139,#18140,#18141,#18142,#18143,#18144,#18145,#18146,#18147,#18148,
#18149,#18150,#18151,#18152,#18153,#18154,#18155,#18156,#18157,#18158,#18159,
#18160,#18161,#18162,#18163,#18164,#18165,#18166),.UNSPECIFIED.,.F.,.F.,
(4,3,3,3,3,3,3,3,3,3,3,4),(0.,0.0110116267986798,0.0198365927950272,0.0393688637311641,
0.0455583406049715,0.0493231568143408,0.0527005792502689,0.056916196494854,
0.0651768568763584,0.0788461297337949,0.0828398890027903,0.100882854089343),
 .UNSPECIFIED.);
#564=B_SPLINE_CURVE_WITH_KNOTS('',3,(#18284,#18285,#18286,#18287,#18288,
#18289,#18290,#18291,#18292,#18293,#18294,#18295,#18296,#18297),
 .UNSPECIFIED.,.F.,.F.,(4,1,1,1,1,1,1,1,1,2,4),(-0.889886066635509,-0.843971490026765,
-0.78979558357151,-0.749163653730069,-0.681443770661001,-0.654355817433373,
-0.627267864205746,-0.600179910978118,-0.573091957750491,-0.464740144839981,
-0.44137654239973),.UNSPECIFIED.);
#565=B_SPLINE_CURVE_WITH_KNOTS('',3,(#18299,#18300,#18301,#18302,#18303,
#18304,#18305,#18306,#18307,#18308,#18309,#18310),.UNSPECIFIED.,.F.,.F.,
(4,2,2,2,2,4),(0.,0.0358257028990328,0.131952299625094,0.148884451735932,
0.157379698574708,0.16223106694039),.UNSPECIFIED.);
#566=B_SPLINE_CURVE_WITH_KNOTS('',3,(#18312,#18313,#18314,#18315),
 .UNSPECIFIED.,.F.,.F.,(4,4),(0.549999999941368,1.),.UNSPECIFIED.);
#567=B_SPLINE_CURVE_WITH_KNOTS('',3,(#18317,#18318,#18319,#18320,#18321,
#18322,#18323,#18324,#18325,#18326,#18327,#18328,#18329,#18330,#18331,#18332),
 .UNSPECIFIED.,.F.,.F.,(4,1,2,1,1,1,1,1,1,1,1,1,4),(0.310721506882948,0.387730825861464,
0.464740144839981,0.573091957750491,0.600179910978118,0.627267864205746,
0.654355817433373,0.681443770661001,0.749163653730069,0.78979558357151,
0.843971490026765,0.89814739648202,0.929489890414014),.UNSPECIFIED.);
#568=B_SPLINE_CURVE_WITH_KNOTS('',3,(#18333,#18334,#18335,#18336,#18337,
#18338,#18339,#18340,#18341,#18342,#18343,#18344,#18345,#18346,#18347,#18348,
#18349),.UNSPECIFIED.,.F.,.F.,(4,1,1,1,1,1,1,1,1,1,1,1,1,1,4),(0.929489890414014,
0.952323302937276,1.00649920939253,1.06067511584779,1.11485102230304,1.1690269287583,
1.22320283521355,1.26383476505499,1.33155464812406,1.35864260135169,1.38573055457932,
1.41281850780694,1.43990646103457,1.49408236748983,1.54825827394508),
 .UNSPECIFIED.);
#569=B_SPLINE_CURVE_WITH_KNOTS('',3,(#18351,#18352,#18353,#18354,#18355,
#18356,#18357,#18358,#18359,#18360,#18361,#18362,#18363,#18364),
 .UNSPECIFIED.,.F.,.F.,(4,2,2,2,2,2,4),(0.16223106694039,0.163967550885131,
0.171180716857468,0.182777598096348,0.205784524866042,0.262730804446443,
0.324280670363194),.UNSPECIFIED.);
#570=B_SPLINE_CURVE_WITH_KNOTS('',3,(#18365,#18366,#18367,#18368,#18369,
#18370,#18371,#18372,#18373,#18374,#18375,#18376,#18377,#18378),
 .UNSPECIFIED.,.F.,.F.,(4,1,1,1,1,1,1,1,1,1,1,4),(-1.4176032384283,-1.41281850780694,
-1.38573055457932,-1.35864260135169,-1.33155464812406,-1.26383476505499,
-1.22320283521355,-1.1690269287583,-1.11485102230304,-1.06067511584779,
-1.00649920939253,-0.969093714192518),.UNSPECIFIED.);
#571=B_SPLINE_CURVE_WITH_KNOTS('',3,(#18384,#18385,#18386,#18387,#18388,
#18389,#18390,#18391,#18392,#18393,#18394,#18395),.UNSPECIFIED.,.F.,.F.,
(4,1,1,1,1,1,1,2,4),(-1.50954599357819,-1.43295998077967,-1.38938999215504,
-1.34582000353042,-1.25868002628116,-1.21511003765654,-1.17154004903191,
-1.08440007178266,-1.06103646934241),.UNSPECIFIED.);
#572=B_SPLINE_CURVE_WITH_KNOTS('',3,(#18398,#18399,#18400,#18401,#18402,
#18403,#18404,#18405,#18406,#18407,#18408,#18409,#18410,#18411),
 .UNSPECIFIED.,.F.,.F.,(4,1,1,1,2,2,1,1,1,4),(-2.03726316537097,-2.03275764211163,
-2.01344899085789,-1.93621438584296,-1.85897978082803,-1.78151988977668,
-1.71616490683974,-1.69437991252743,-1.60723993527817,-1.58875364113519),
 .UNSPECIFIED.);
#573=B_SPLINE_CURVE_WITH_KNOTS('',3,(#18417,#18418,#18419,#18420,#18421,
#18422,#18423,#18424,#18425,#18426),.UNSPECIFIED.,.F.,.F.,(4,2,2,2,4),(0.,
0.0782721603764034,0.156544320752807,0.234729089704077,0.312913858655347),
 .UNSPECIFIED.);
#574=B_SPLINE_CURVE_WITH_KNOTS('',3,(#18427,#18428,#18429,#18430,#18431,
#18432,#18433,#18434,#18435,#18436,#18437,#18438,#18439,#18440,#18441,#18442,
#18443,#18444,#18445,#18446,#18447,#18448,#18449,#18450,#18451,#18452),
 .UNSPECIFIED.,.F.,.F.,(4,2,2,2,2,2,2,2,2,2,2,2,4),(0.312913858655347,0.391098627606618,
0.469283396557888,0.547555556934292,0.625827717310695,0.704099877687098,
0.782372038063502,0.860556807014772,0.938741575966043,1.01692634491731,
1.09511111386858,1.17338327424499,1.25165543462139),.UNSPECIFIED.);
#575=B_SPLINE_CURVE_WITH_KNOTS('',3,(#18566,#18567,#18568,#18569,#18570,
#18571,#18572,#18573,#18574,#18575,#18576,#18577),.UNSPECIFIED.,.F.,.F.,
(4,2,2,2,2,4),(0.,0.0358257028990433,0.131952299625135,0.148884451735976,
0.157379698574799,0.162231066940522),.UNSPECIFIED.);
#576=B_SPLINE_CURVE_WITH_KNOTS('',3,(#18579,#18580,#18581,#18582),
 .UNSPECIFIED.,.F.,.F.,(4,4),(0.549999999941368,1.),.UNSPECIFIED.);
#577=B_SPLINE_CURVE_WITH_KNOTS('',3,(#18584,#18585,#18586,#18587,#18588,
#18589,#18590,#18591,#18592,#18593,#18594,#18595,#18596,#18597),
 .UNSPECIFIED.,.F.,.F.,(4,1,2,1,1,1,1,1,1,1,4),(0.930381433825624,1.00739075280414,
1.08440007178266,1.17154004903191,1.21511003765654,1.25868002628116,1.34582000353042,
1.38938999215504,1.43295998077967,1.52009995802892,1.54914981735669),
 .UNSPECIFIED.);
#578=B_SPLINE_CURVE_WITH_KNOTS('',3,(#18598,#18599,#18600,#18601,#18602,
#18603,#18604,#18605,#18606,#18607,#18608,#18609,#18610,#18611,#18612,#18613,
#18614,#18615),.UNSPECIFIED.,.F.,.F.,(4,1,1,1,1,1,2,2,1,1,1,1,1,4),(1.54914981735669,
1.56366994665355,1.58545494096586,1.60723993527817,1.69437991252743,1.71616490683974,
1.78151988977668,1.85897978082803,1.93621438584296,2.01344899085789,2.03275764211163,
2.05206629336536,2.09068359587282,2.16791820088776),.UNSPECIFIED.);
#579=B_SPLINE_CURVE_WITH_KNOTS('',3,(#18616,#18617,#18618,#18619,#18620,
#18621,#18622,#18623,#18624,#18625,#18626,#18627,#18628,#18629),
 .UNSPECIFIED.,.F.,.F.,(4,2,2,2,2,2,4),(0.162231066940522,0.163967550885278,
0.171180716857662,0.182777598096494,0.205784524865831,0.262730804445425,
0.324280670361326),.UNSPECIFIED.);
#580=B_SPLINE_CURVE_WITH_KNOTS('',3,(#18633,#18634,#18635,#18636,#18637,
#18638,#18639,#18640,#18641,#18642,#18643,#18644,#18645,#18646,#18647,#18648,
#18649,#18650,#18651,#18652,#18653,#18654,#18655,#18656,#18657,#18658),
 .UNSPECIFIED.,.F.,.F.,(4,2,2,2,2,2,2,2,2,2,2,2,4),(0.,0.0782721603764034,
0.156544320752807,0.234729089704077,0.312913858655348,0.391098627606618,
0.469283396557888,0.547555556934292,0.625827717310695,0.704099877687099,
0.782372038063502,0.860556807014772,0.938741575966043),.UNSPECIFIED.);
#581=B_SPLINE_CURVE_WITH_KNOTS('',3,(#18659,#18660,#18661,#18662,#18663,
#18664,#18665,#18666,#18667,#18668),.UNSPECIFIED.,.F.,.F.,(4,2,2,2,4),(0.938741575966043,
1.01692634491731,1.09511111386858,1.17338327424499,1.25165543462139),
 .UNSPECIFIED.);
#582=B_SPLINE_CURVE_WITH_KNOTS('',3,(#18700,#18701,#18702,#18703,#18704,
#18705),.UNSPECIFIED.,.F.,.F.,(4,2,4),(0.,0.138460176945389,0.254919406868435),
 .UNSPECIFIED.);
#583=B_SPLINE_CURVE_WITH_KNOTS('',3,(#18706,#18707,#18708,#18709,#18710,
#18711),.UNSPECIFIED.,.F.,.F.,(4,2,4),(0.0638119305867456,0.434740434623819,
0.895232561311265),.UNSPECIFIED.);
#584=B_SPLINE_CURVE_WITH_KNOTS('',3,(#18712,#18713,#18714,#18715,#18716,
#18717,#18718,#18719),.UNSPECIFIED.,.F.,.F.,(4,2,2,4),(0.0746811865707125,
0.397508022614213,0.744535688298142,1.03619555646955),.UNSPECIFIED.);
#585=B_SPLINE_CURVE_WITH_KNOTS('',3,(#18746,#18747,#18748,#18749,#18750,
#18751,#18752,#18753),.UNSPECIFIED.,.F.,.F.,(4,2,2,4),(0.0544345524991837,
0.140376841744982,0.193303927754724,0.23329596220082),.UNSPECIFIED.);
#586=B_SPLINE_CURVE_WITH_KNOTS('',3,(#18754,#18755,#18756,#18757,#18758,
#18759,#18760,#18761),.UNSPECIFIED.,.F.,.F.,(4,2,2,4),(0.15440517711793,
0.43827181462838,0.790258491635714,1.12994605591353),.UNSPECIFIED.);
#587=B_SPLINE_CURVE_WITH_KNOTS('',3,(#18762,#18763,#18764,#18765,#18766,
#18767),.UNSPECIFIED.,.F.,.F.,(4,2,4),(0.0638119305867456,0.434740434623819,
0.895232561311264),.UNSPECIFIED.);
#588=B_SPLINE_CURVE_WITH_KNOTS('',3,(#18784,#18785,#18786,#18787,#18788,
#18789,#18790),.UNSPECIFIED.,.F.,.F.,(4,3,4),(0.,0.0653793053833038,0.130355487793338),
 .UNSPECIFIED.);
#589=B_SPLINE_CURVE_WITH_KNOTS('',3,(#18794,#18795,#18796,#18797,#18798,
#18799,#18800,#18801),.UNSPECIFIED.,.F.,.F.,(4,2,2,4),(0.0746811865707133,
0.397508022614224,0.744535688298146,1.0361955564692),.UNSPECIFIED.);
#590=B_SPLINE_CURVE_WITH_KNOTS('',3,(#18804,#18805,#18806,#18807,#18808,
#18809,#18810,#18811),.UNSPECIFIED.,.F.,.F.,(4,2,2,4),(0.15440517711793,
0.438271814628377,0.790258491635718,1.12994605591353),.UNSPECIFIED.);
#591=B_SPLINE_CURVE_WITH_KNOTS('',3,(#18839,#18840,#18841,#18842,#18843,
#18844),.UNSPECIFIED.,.F.,.F.,(4,2,4),(0.,0.138460176942891,0.254919406877601),
 .UNSPECIFIED.);
#592=B_SPLINE_CURVE_WITH_KNOTS('',3,(#18845,#18846,#18847,#18848,#18849,
#18850),.UNSPECIFIED.,.F.,.F.,(4,2,4),(0.0638119305867455,0.434740434623819,
0.895232561311264),.UNSPECIFIED.);
#593=B_SPLINE_CURVE_WITH_KNOTS('',3,(#18851,#18852,#18853,#18854,#18855,
#18856,#18857,#18858),.UNSPECIFIED.,.F.,.F.,(4,2,2,4),(0.0746811865707128,
0.397508022614225,0.744535688298148,1.03619555646854),.UNSPECIFIED.);
#594=B_SPLINE_CURVE_WITH_KNOTS('',3,(#18884,#18885,#18886,#18887,#18888,
#18889,#18890,#18891),.UNSPECIFIED.,.F.,.F.,(4,2,2,4),(0.0544345524999985,
0.140376841748909,0.193303927764524,0.233295962216222),.UNSPECIFIED.);
#595=B_SPLINE_CURVE_WITH_KNOTS('',3,(#18892,#18893,#18894,#18895,#18896,
#18897),.UNSPECIFIED.,.F.,.F.,(4,2,4),(0.0638119305867455,0.434740434623819,
0.895232561311264),.UNSPECIFIED.);
#596=B_SPLINE_CURVE_WITH_KNOTS('',3,(#18914,#18915,#18916,#18917,#18918,
#18919,#18920),.UNSPECIFIED.,.F.,.F.,(4,3,4),(0.,0.0653793053833002,0.130355487793372),
 .UNSPECIFIED.);
#597=B_SPLINE_CURVE_WITH_KNOTS('',3,(#18923,#18924,#18925,#18926,#18927,
#18928,#18929,#18930),.UNSPECIFIED.,.F.,.F.,(4,2,2,4),(0.154405177117932,
0.438271814628394,0.790258491635738,1.12994605591355),.UNSPECIFIED.);
#598=B_SPLINE_CURVE_WITH_KNOTS('',3,(#18958,#18959,#18960,#18961,#18962,
#18963),.UNSPECIFIED.,.F.,.F.,(4,2,4),(0.,0.138460176943918,0.254919406860805),
 .UNSPECIFIED.);
#599=B_SPLINE_CURVE_WITH_KNOTS('',3,(#18964,#18965,#18966,#18967,#18968,
#18969),.UNSPECIFIED.,.F.,.F.,(4,2,4),(0.0638119305867456,0.434740434623819,
0.895232561311265),.UNSPECIFIED.);
#600=B_SPLINE_CURVE_WITH_KNOTS('',3,(#18970,#18971,#18972,#18973,#18974,
#18975,#18976,#18977),.UNSPECIFIED.,.F.,.F.,(4,2,2,4),(0.0746811865707128,
0.397508022614222,0.744535688298131,1.03619555646937),.UNSPECIFIED.);
#601=B_SPLINE_CURVE_WITH_KNOTS('',3,(#19003,#19004,#19005,#19006,#19007,
#19008,#19009,#19010),.UNSPECIFIED.,.F.,.F.,(4,2,2,4),(0.0544345524991458,
0.140376841744735,0.193303927754458,0.233295962201587),.UNSPECIFIED.);
#602=B_SPLINE_CURVE_WITH_KNOTS('',3,(#19011,#19012,#19013,#19014,#19015,
#19016),.UNSPECIFIED.,.F.,.F.,(4,2,4),(0.0638119305867456,0.434740434623819,
0.895232561311265),.UNSPECIFIED.);
#603=B_SPLINE_CURVE_WITH_KNOTS('',3,(#19033,#19034,#19035,#19036,#19037,
#19038,#19039),.UNSPECIFIED.,.F.,.F.,(4,3,4),(0.,0.0653793053832705,0.130355487793285),
 .UNSPECIFIED.);
#604=B_SPLINE_CURVE_WITH_KNOTS('',3,(#19042,#19043,#19044,#19045,#19046,
#19047,#19048,#19049),.UNSPECIFIED.,.F.,.F.,(4,2,2,4),(0.15440517711793,
0.438271814628378,0.790258491635719,1.12994605591353),.UNSPECIFIED.);
#605=B_SPLINE_CURVE_WITH_KNOTS('',3,(#19077,#19078,#19079,#19080,#19081,
#19082),.UNSPECIFIED.,.F.,.F.,(4,2,4),(0.,0.138460176945285,0.254919406866285),
 .UNSPECIFIED.);
#606=B_SPLINE_CURVE_WITH_KNOTS('',3,(#19083,#19084,#19085,#19086,#19087,
#19088),.UNSPECIFIED.,.F.,.F.,(4,2,4),(0.0638119305867456,0.434740434623819,
0.895232561311265),.UNSPECIFIED.);
#607=B_SPLINE_CURVE_WITH_KNOTS('',3,(#19089,#19090,#19091,#19092,#19093,
#19094,#19095,#19096),.UNSPECIFIED.,.F.,.F.,(4,2,2,4),(0.0746811865707126,
0.397508022614211,0.744535688298121,1.05488349691751),.UNSPECIFIED.);
#608=B_SPLINE_CURVE_WITH_KNOTS('',3,(#19122,#19123,#19124,#19125,#19126,
#19127,#19128,#19129),.UNSPECIFIED.,.F.,.F.,(4,2,2,4),(0.0544345524985586,
0.140376841742248,0.193303927756487,0.233295962206935),.UNSPECIFIED.);
#609=B_SPLINE_CURVE_WITH_KNOTS('',3,(#19130,#19131,#19132,#19133,#19134,
#19135),.UNSPECIFIED.,.F.,.F.,(4,2,4),(0.0638119305867456,0.434740434623819,
0.895232561311265),.UNSPECIFIED.);
#610=B_SPLINE_CURVE_WITH_KNOTS('',3,(#19152,#19153,#19154,#19155,#19156,
#19157,#19158),.UNSPECIFIED.,.F.,.F.,(4,3,4),(0.,0.0653793053832869,0.130355487793285),
 .UNSPECIFIED.);
#611=B_SPLINE_CURVE_WITH_KNOTS('',3,(#19161,#19162,#19163,#19164,#19165,
#19166,#19167,#19168),.UNSPECIFIED.,.F.,.F.,(4,2,2,4),(0.0774162478443013,
0.414979417786432,0.760655521250469,1.05194916247838),.UNSPECIFIED.);
#612=B_SPLINE_CURVE_WITH_KNOTS('',3,(#19196,#19197,#19198,#19199,#19200,
#19201),.UNSPECIFIED.,.F.,.F.,(4,2,4),(0.,0.138460176945226,0.254919406867686),
 .UNSPECIFIED.);
#613=B_SPLINE_CURVE_WITH_KNOTS('',3,(#19202,#19203,#19204,#19205,#19206,
#19207),.UNSPECIFIED.,.F.,.F.,(4,2,4),(0.0638119305867456,0.434740434623819,
0.895232561311265),.UNSPECIFIED.);
#614=B_SPLINE_CURVE_WITH_KNOTS('',3,(#19208,#19209,#19210,#19211,#19212,
#19213,#19214,#19215),.UNSPECIFIED.,.F.,.F.,(4,2,2,4),(0.0746811865707126,
0.397508022614209,0.744535688298118,1.03619555646857),.UNSPECIFIED.);
#615=B_SPLINE_CURVE_WITH_KNOTS('',3,(#19241,#19242,#19243,#19244,#19245,
#19246,#19247,#19248),.UNSPECIFIED.,.F.,.F.,(4,2,2,4),(0.0544345524990915,
0.140376841744593,0.193303927757736,0.233295962205675),.UNSPECIFIED.);
#616=B_SPLINE_CURVE_WITH_KNOTS('',3,(#19249,#19250,#19251,#19252,#19253,
#19254),.UNSPECIFIED.,.F.,.F.,(4,2,4),(0.0638119305867457,0.434740434623819,
0.895232561311264),.UNSPECIFIED.);
#617=B_SPLINE_CURVE_WITH_KNOTS('',3,(#19271,#19272,#19273,#19274,#19275,
#19276,#19277),.UNSPECIFIED.,.F.,.F.,(4,3,4),(0.,0.0653793053833536,0.130355487793441),
 .UNSPECIFIED.);
#618=B_SPLINE_CURVE_WITH_KNOTS('',3,(#19280,#19281,#19282,#19283,#19284,
#19285,#19286,#19287),.UNSPECIFIED.,.F.,.F.,(4,2,2,4),(0.154405177117923,
0.438271814628353,0.790258491635649,1.1299460559134),.UNSPECIFIED.);
#619=B_SPLINE_CURVE_WITH_KNOTS('',3,(#19315,#19316,#19317,#19318,#19319,
#19320),.UNSPECIFIED.,.F.,.F.,(4,2,4),(0.,0.138460176945371,0.254919406866122),
 .UNSPECIFIED.);
#620=B_SPLINE_CURVE_WITH_KNOTS('',3,(#19321,#19322,#19323,#19324,#19325,
#19326),.UNSPECIFIED.,.F.,.F.,(4,2,4),(0.0638119305867456,0.434740434623819,
0.895232561311265),.UNSPECIFIED.);
#621=B_SPLINE_CURVE_WITH_KNOTS('',3,(#19327,#19328,#19329,#19330,#19331,
#19332,#19333,#19334),.UNSPECIFIED.,.F.,.F.,(4,2,2,4),(0.0746811865707114,
0.397508022614213,0.744535688298102,1.03619555646808),.UNSPECIFIED.);
#622=B_SPLINE_CURVE_WITH_KNOTS('',3,(#19360,#19361,#19362,#19363,#19364,
#19365,#19366,#19367),.UNSPECIFIED.,.F.,.F.,(4,2,2,4),(0.0544345524988946,
0.140376841743774,0.193303927754125,0.233295962200619),.UNSPECIFIED.);
#623=B_SPLINE_CURVE_WITH_KNOTS('',3,(#19368,#19369,#19370,#19371,#19372,
#19373),.UNSPECIFIED.,.F.,.F.,(4,2,4),(0.0638119305867456,0.434740434623819,
0.895232561311264),.UNSPECIFIED.);
#624=B_SPLINE_CURVE_WITH_KNOTS('',3,(#19390,#19391,#19392,#19393,#19394,
#19395,#19396),.UNSPECIFIED.,.F.,.F.,(4,3,4),(0.,0.0653793053832619,0.130355487793235),
 .UNSPECIFIED.);
#625=B_SPLINE_CURVE_WITH_KNOTS('',3,(#19399,#19400,#19401,#19402,#19403,
#19404,#19405,#19406),.UNSPECIFIED.,.F.,.F.,(4,2,2,4),(0.154405177117934,
0.4382718146284,0.790258491635752,1.12994605591358),.UNSPECIFIED.);
#626=B_SPLINE_CURVE_WITH_KNOTS('',3,(#19434,#19435,#19436,#19437,#19438,
#19439),.UNSPECIFIED.,.F.,.F.,(4,2,4),(0.,0.138460176943452,0.25491940687479),
 .UNSPECIFIED.);
#627=B_SPLINE_CURVE_WITH_KNOTS('',3,(#19440,#19441,#19442,#19443,#19444,
#19445),.UNSPECIFIED.,.F.,.F.,(4,2,4),(0.0638119305867456,0.434740434623819,
0.895232561311265),.UNSPECIFIED.);
#628=B_SPLINE_CURVE_WITH_KNOTS('',3,(#19446,#19447,#19448,#19449,#19450,
#19451,#19452,#19453),.UNSPECIFIED.,.F.,.F.,(4,2,2,4),(0.0746811865707127,
0.397508022614219,0.744535688298134,1.0361955564692),.UNSPECIFIED.);
#629=B_SPLINE_CURVE_WITH_KNOTS('',3,(#19479,#19480,#19481,#19482,#19483,
#19484,#19485,#19486),.UNSPECIFIED.,.F.,.F.,(4,2,2,4),(0.0544345524985935,
0.140376841742227,0.193303927751676,0.233295962196035),.UNSPECIFIED.);
#630=B_SPLINE_CURVE_WITH_KNOTS('',3,(#19487,#19488,#19489,#19490,#19491,
#19492),.UNSPECIFIED.,.F.,.F.,(4,2,4),(0.0638119305867456,0.434740434623819,
0.895232561311264),.UNSPECIFIED.);
#631=B_SPLINE_CURVE_WITH_KNOTS('',3,(#19509,#19510,#19511,#19512,#19513,
#19514,#19515),.UNSPECIFIED.,.F.,.F.,(4,3,4),(0.,0.0653793053833638,0.130355487793505),
 .UNSPECIFIED.);
#632=B_SPLINE_CURVE_WITH_KNOTS('',3,(#19518,#19519,#19520,#19521,#19522,
#19523,#19524,#19525),.UNSPECIFIED.,.F.,.F.,(4,2,2,4),(0.154405177117939,
0.438271814628415,0.790258491635773,1.12994605591359),.UNSPECIFIED.);
#633=B_SPLINE_CURVE_WITH_KNOTS('',3,(#19553,#19554,#19555,#19556,#19557,
#19558),.UNSPECIFIED.,.F.,.F.,(4,2,4),(0.,0.138460176943768,0.254919406861752),
 .UNSPECIFIED.);
#634=B_SPLINE_CURVE_WITH_KNOTS('',3,(#19559,#19560,#19561,#19562,#19563,
#19564),.UNSPECIFIED.,.F.,.F.,(4,2,4),(0.0638119305867455,0.434740434623819,
0.895232561311264),.UNSPECIFIED.);
#635=B_SPLINE_CURVE_WITH_KNOTS('',3,(#19565,#19566,#19567,#19568,#19569,
#19570,#19571,#19572),.UNSPECIFIED.,.F.,.F.,(4,2,2,4),(0.074681186570713,
0.397508022614234,0.744535688298142,1.03619555646862),.UNSPECIFIED.);
#636=B_SPLINE_CURVE_WITH_KNOTS('',3,(#19598,#19599,#19600,#19601,#19602,
#19603,#19604,#19605),.UNSPECIFIED.,.F.,.F.,(4,2,2,4),(0.0544345524996551,
0.140376841747112,0.193303927760047,0.233295962211347),.UNSPECIFIED.);
#637=B_SPLINE_CURVE_WITH_KNOTS('',3,(#19606,#19607,#19608,#19609,#19610,
#19611),.UNSPECIFIED.,.F.,.F.,(4,2,4),(0.0638119305867455,0.434740434623819,
0.895232561311264),.UNSPECIFIED.);
#638=B_SPLINE_CURVE_WITH_KNOTS('',3,(#19628,#19629,#19630,#19631,#19632,
#19633,#19634),.UNSPECIFIED.,.F.,.F.,(4,3,4),(0.,0.065379305383271,0.130355487793261),
 .UNSPECIFIED.);
#639=B_SPLINE_CURVE_WITH_KNOTS('',3,(#19637,#19638,#19639,#19640,#19641,
#19642,#19643,#19644),.UNSPECIFIED.,.F.,.F.,(4,2,2,4),(0.154405177117931,
0.43827181462838,0.790258491635724,1.12994605591354),.UNSPECIFIED.);
#640=B_SPLINE_CURVE_WITH_KNOTS('',3,(#19672,#19673,#19674,#19675,#19676,
#19677),.UNSPECIFIED.,.F.,.F.,(4,2,4),(0.,0.13846017694485,0.254919406873115),
 .UNSPECIFIED.);
#641=B_SPLINE_CURVE_WITH_KNOTS('',3,(#19678,#19679,#19680,#19681,#19682,
#19683),.UNSPECIFIED.,.F.,.F.,(4,2,4),(0.0638119305867456,0.434740434623819,
0.895232561311265),.UNSPECIFIED.);
#642=B_SPLINE_CURVE_WITH_KNOTS('',3,(#19684,#19685,#19686,#19687,#19688,
#19689,#19690,#19691),.UNSPECIFIED.,.F.,.F.,(4,2,2,4),(0.0746811865707127,
0.397508022614212,0.74453568829812,1.05488349691753),.UNSPECIFIED.);
#643=B_SPLINE_CURVE_WITH_KNOTS('',3,(#19717,#19718,#19719,#19720,#19721,
#19722,#19723,#19724),.UNSPECIFIED.,.F.,.F.,(4,2,2,4),(0.0544345524992758,
0.140376841745509,0.193303927759893,0.233295962209951),.UNSPECIFIED.);
#644=B_SPLINE_CURVE_WITH_KNOTS('',3,(#19725,#19726,#19727,#19728,#19729,
#19730),.UNSPECIFIED.,.F.,.F.,(4,2,4),(0.0638119305867456,0.434740434623819,
0.895232561311265),.UNSPECIFIED.);
#645=B_SPLINE_CURVE_WITH_KNOTS('',3,(#19747,#19748,#19749,#19750,#19751,
#19752,#19753),.UNSPECIFIED.,.F.,.F.,(4,3,4),(0.,0.0653793053833319,0.130355487793411),
 .UNSPECIFIED.);
#646=B_SPLINE_CURVE_WITH_KNOTS('',3,(#19756,#19757,#19758,#19759,#19760,
#19761,#19762,#19763),.UNSPECIFIED.,.F.,.F.,(4,2,2,4),(0.0774162478442982,
0.414979417786394,0.760655521250395,1.05194916247827),.UNSPECIFIED.);
#647=B_SPLINE_CURVE_WITH_KNOTS('',3,(#19791,#19792,#19793,#19794,#19795,
#19796),.UNSPECIFIED.,.F.,.F.,(4,2,4),(0.,0.13846017694524,0.209756131428923),
 .UNSPECIFIED.);
#648=B_SPLINE_CURVE_WITH_KNOTS('',3,(#19797,#19798,#19799,#19800,#19801,
#19802),.UNSPECIFIED.,.F.,.F.,(4,2,4),(0.0638119305867456,0.434740434623819,
0.895232561311265),.UNSPECIFIED.);
#649=B_SPLINE_CURVE_WITH_KNOTS('',3,(#19804,#19805,#19806,#19807,#19808,
#19809,#19810,#19811),.UNSPECIFIED.,.F.,.F.,(4,2,2,4),(0.0746811865707122,
0.397508022614215,0.744535688298118,1.03619555646847),.UNSPECIFIED.);
#650=B_SPLINE_CURVE_WITH_KNOTS('',3,(#19812,#19813,#19814,#19815),
 .UNSPECIFIED.,.F.,.F.,(4,4),(0.209756131428923,0.254919406867736),
 .UNSPECIFIED.);
#651=B_SPLINE_CURVE_WITH_KNOTS('',3,(#19841,#19842,#19843,#19844,#19845,
#19846,#19847,#19848),.UNSPECIFIED.,.F.,.F.,(4,2,2,4),(0.0544345524990686,
0.140376841744483,0.193303927757129,0.233295962204701),.UNSPECIFIED.);
#652=B_SPLINE_CURVE_WITH_KNOTS('',3,(#19849,#19850,#19851,#19852,#19853,
#19854),.UNSPECIFIED.,.F.,.F.,(4,2,4),(0.0638119305867457,0.434740434623819,
0.895232561311264),.UNSPECIFIED.);
#653=B_SPLINE_CURVE_WITH_KNOTS('',3,(#19871,#19872,#19873,#19874,#19875,
#19876,#19877),.UNSPECIFIED.,.F.,.F.,(4,3,4),(0.,0.0653793053833073,0.130355487793357),
 .UNSPECIFIED.);
#654=B_SPLINE_CURVE_WITH_KNOTS('',3,(#19880,#19881,#19882,#19883,#19884,
#19885,#19886,#19887),.UNSPECIFIED.,.F.,.F.,(4,2,2,4),(0.154405177117928,
0.438271814628368,0.790258491635699,1.12994605591349),.UNSPECIFIED.);
#655=B_SPLINE_CURVE_WITH_KNOTS('',3,(#19915,#19916,#19917,#19918,#19919,
#19920),.UNSPECIFIED.,.F.,.F.,(4,2,4),(0.,0.138460176945471,0.254919406864932),
 .UNSPECIFIED.);
#656=B_SPLINE_CURVE_WITH_KNOTS('',3,(#19921,#19922,#19923,#19924,#19925,
#19926),.UNSPECIFIED.,.F.,.F.,(4,2,4),(0.0638119305867457,0.434740434623819,
0.895232561311265),.UNSPECIFIED.);
#657=B_SPLINE_CURVE_WITH_KNOTS('',3,(#19927,#19928,#19929,#19930,#19931,
#19932,#19933,#19934),.UNSPECIFIED.,.F.,.F.,(4,2,2,4),(0.0746811865707118,
0.39750802261421,0.744535688298092,1.03619555646858),.UNSPECIFIED.);
#658=B_SPLINE_CURVE_WITH_KNOTS('',3,(#19960,#19961,#19962,#19963,#19964,
#19965,#19966,#19967),.UNSPECIFIED.,.F.,.F.,(4,2,2,4),(0.0544345524998506,
0.140376841748323,0.193303927766303,0.233295962218452),.UNSPECIFIED.);
#659=B_SPLINE_CURVE_WITH_KNOTS('',3,(#19968,#19969,#19970,#19971,#19972,
#19973),.UNSPECIFIED.,.F.,.F.,(4,2,4),(0.0638119305867456,0.434740434623819,
0.895232561311265),.UNSPECIFIED.);
#660=B_SPLINE_CURVE_WITH_KNOTS('',3,(#19990,#19991,#19992,#19993,#19994,
#19995,#19996),.UNSPECIFIED.,.F.,.F.,(4,3,4),(0.,0.0653793053833078,0.130355487793348),
 .UNSPECIFIED.);
#661=B_SPLINE_CURVE_WITH_KNOTS('',3,(#19999,#20000,#20001,#20002,#20003,
#20004,#20005,#20006),.UNSPECIFIED.,.F.,.F.,(4,2,2,4),(0.154405177117931,
0.438271814628383,0.790258491635722,1.12994605591352),.UNSPECIFIED.);
#662=B_SPLINE_CURVE_WITH_KNOTS('',3,(#20034,#20035,#20036,#20037,#20038,
#20039),.UNSPECIFIED.,.F.,.F.,(4,2,4),(0.,0.138460176943519,0.254919406873928),
 .UNSPECIFIED.);
#663=B_SPLINE_CURVE_WITH_KNOTS('',3,(#20040,#20041,#20042,#20043,#20044,
#20045),.UNSPECIFIED.,.F.,.F.,(4,2,4),(0.0638119305867456,0.434740434623819,
0.895232561311265),.UNSPECIFIED.);
#664=B_SPLINE_CURVE_WITH_KNOTS('',3,(#20046,#20047,#20048,#20049,#20050,
#20051,#20052,#20053),.UNSPECIFIED.,.F.,.F.,(4,2,2,4),(0.0746811865707111,
0.397508022614208,0.744535688298079,1.036195556468),.UNSPECIFIED.);
#665=B_SPLINE_CURVE_WITH_KNOTS('',3,(#20079,#20080,#20081,#20082,#20083,
#20084,#20085,#20086),.UNSPECIFIED.,.F.,.F.,(4,2,2,4),(0.0544345524985954,
0.140376841742234,0.193303927751678,0.233295962196024),.UNSPECIFIED.);
#666=B_SPLINE_CURVE_WITH_KNOTS('',3,(#20087,#20088,#20089,#20090,#20091,
#20092),.UNSPECIFIED.,.F.,.F.,(4,2,4),(0.0638119305867456,0.434740434623819,
0.895232561311264),.UNSPECIFIED.);
#667=B_SPLINE_CURVE_WITH_KNOTS('',3,(#20109,#20110,#20111,#20112,#20113,
#20114,#20115),.UNSPECIFIED.,.F.,.F.,(4,3,4),(0.,0.0653793053833565,0.130355487793492),
 .UNSPECIFIED.);
#668=B_SPLINE_CURVE_WITH_KNOTS('',3,(#20118,#20119,#20120,#20121,#20122,
#20123,#20124,#20125),.UNSPECIFIED.,.F.,.F.,(4,2,2,4),(0.15440517711794,
0.438271814628416,0.790258491635786,1.12994605591364),.UNSPECIFIED.);
#669=B_SPLINE_CURVE_WITH_KNOTS('',3,(#20153,#20154,#20155,#20156,#20157,
#20158),.UNSPECIFIED.,.F.,.F.,(4,2,4),(0.,0.138460176943852,0.254919406858792),
 .UNSPECIFIED.);
#670=B_SPLINE_CURVE_WITH_KNOTS('',3,(#20159,#20160,#20161,#20162,#20163,
#20164),.UNSPECIFIED.,.F.,.F.,(4,2,4),(0.0638119305867455,0.434740434623819,
0.895232561311264),.UNSPECIFIED.);
#671=B_SPLINE_CURVE_WITH_KNOTS('',3,(#20165,#20166,#20167,#20168,#20169,
#20170,#20171,#20172),.UNSPECIFIED.,.F.,.F.,(4,2,2,4),(0.074681186570714,
0.397508022614236,0.744535688298161,1.03619555646797),.UNSPECIFIED.);
#672=B_SPLINE_CURVE_WITH_KNOTS('',3,(#20198,#20199,#20200,#20201,#20202,
#20203,#20204,#20205),.UNSPECIFIED.,.F.,.F.,(4,2,2,4),(0.054434552499654,
0.140376841747107,0.193303927760024,0.233295962211313),.UNSPECIFIED.);
#673=B_SPLINE_CURVE_WITH_KNOTS('',3,(#20206,#20207,#20208,#20209,#20210,
#20211),.UNSPECIFIED.,.F.,.F.,(4,2,4),(0.0638119305867455,0.434740434623819,
0.895232561311264),.UNSPECIFIED.);
#674=B_SPLINE_CURVE_WITH_KNOTS('',3,(#20228,#20229,#20230,#20231,#20232,
#20233,#20234),.UNSPECIFIED.,.F.,.F.,(4,3,4),(0.,0.0653793053832257,0.130355487793195),
 .UNSPECIFIED.);
#675=B_SPLINE_CURVE_WITH_KNOTS('',3,(#20237,#20238,#20239,#20240,#20241,
#20242,#20243,#20244),.UNSPECIFIED.,.F.,.F.,(4,2,2,4),(0.154405177117938,
0.438271814628411,0.790258491635778,1.12994605591362),.UNSPECIFIED.);
#676=B_SPLINE_CURVE_WITH_KNOTS('',3,(#20272,#20273,#20274,#20275,#20276,
#20277),.UNSPECIFIED.,.F.,.F.,(4,2,4),(0.,0.138460176944659,0.254919406872703),
 .UNSPECIFIED.);
#677=B_SPLINE_CURVE_WITH_KNOTS('',3,(#20278,#20279,#20280,#20281,#20282,
#20283),.UNSPECIFIED.,.F.,.F.,(4,2,4),(0.0638119305867456,0.434740434623819,
0.895232561311265),.UNSPECIFIED.);
#678=B_SPLINE_CURVE_WITH_KNOTS('',3,(#20284,#20285,#20286,#20287,#20288,
#20289,#20290,#20291),.UNSPECIFIED.,.F.,.F.,(4,2,2,4),(0.0746811865707118,
0.397508022614199,0.7445356882981,1.05488349691747),.UNSPECIFIED.);
#679=B_SPLINE_CURVE_WITH_KNOTS('',3,(#20317,#20318,#20319,#20320,#20321,
#20322,#20323,#20324),.UNSPECIFIED.,.F.,.F.,(4,2,2,4),(0.0544345524994541,
0.140376841746265,0.193303927760631,0.2332959622117),.UNSPECIFIED.);
#680=B_SPLINE_CURVE_WITH_KNOTS('',3,(#20325,#20326,#20327,#20328,#20329,
#20330),.UNSPECIFIED.,.F.,.F.,(4,2,4),(0.0638119305867456,0.434740434623819,
0.895232561311265),.UNSPECIFIED.);
#681=B_SPLINE_CURVE_WITH_KNOTS('',3,(#20347,#20348,#20349,#20350,#20351,
#20352,#20353),.UNSPECIFIED.,.F.,.F.,(4,3,4),(0.,0.0653793053833301,0.130355487793397),
 .UNSPECIFIED.);
#682=B_SPLINE_CURVE_WITH_KNOTS('',3,(#20356,#20357,#20358,#20359,#20360,
#20361,#20362,#20363),.UNSPECIFIED.,.F.,.F.,(4,2,2,4),(0.0774162478442986,
0.414979417786383,0.760655521250363,1.05194916247819),.UNSPECIFIED.);
#683=B_SPLINE_CURVE_WITH_KNOTS('',3,(#20391,#20392,#20393,#20394,#20395,
#20396),.UNSPECIFIED.,.F.,.F.,(4,2,4),(0.,0.138460176945229,0.254919406868124),
 .UNSPECIFIED.);
#684=B_SPLINE_CURVE_WITH_KNOTS('',3,(#20397,#20398,#20399,#20400,#20401,
#20402),.UNSPECIFIED.,.F.,.F.,(4,2,4),(0.0638119305867456,0.434740434623819,
0.895232561311265),.UNSPECIFIED.);
#685=B_SPLINE_CURVE_WITH_KNOTS('',3,(#20403,#20404,#20405,#20406,#20407,
#20408,#20409,#20410),.UNSPECIFIED.,.F.,.F.,(4,2,2,4),(0.0746811865707123,
0.397508022614217,0.744535688298116,1.03619555646925),.UNSPECIFIED.);
#686=B_SPLINE_CURVE_WITH_KNOTS('',3,(#20436,#20437,#20438,#20439,#20440,
#20441,#20442,#20443),.UNSPECIFIED.,.F.,.F.,(4,2,2,4),(0.0544345524990402,
0.140376841744349,0.193303927756099,0.233295962203159),.UNSPECIFIED.);
#687=B_SPLINE_CURVE_WITH_KNOTS('',3,(#20444,#20445,#20446,#20447,#20448,
#20449),.UNSPECIFIED.,.F.,.F.,(4,2,4),(0.0638119305867457,0.434740434623819,
0.895232561311264),.UNSPECIFIED.);
#688=B_SPLINE_CURVE_WITH_KNOTS('',3,(#20466,#20467,#20468,#20469,#20470,
#20471,#20472),.UNSPECIFIED.,.F.,.F.,(4,3,4),(0.,0.0653793053833115,0.130355487793403),
 .UNSPECIFIED.);
#689=B_SPLINE_CURVE_WITH_KNOTS('',3,(#20475,#20476,#20477,#20478,#20479,
#20480,#20481,#20482),.UNSPECIFIED.,.F.,.F.,(4,2,2,4),(0.154405177117932,
0.438271814628382,0.79025849163572,1.12994605591353),.UNSPECIFIED.);
#690=B_SPLINE_CURVE_WITH_KNOTS('',3,(#20510,#20511,#20512,#20513,#20514,
#20515),.UNSPECIFIED.,.F.,.F.,(4,2,4),(0.,0.138460176945405,0.254919406862959),
 .UNSPECIFIED.);
#691=B_SPLINE_CURVE_WITH_KNOTS('',3,(#20516,#20517,#20518,#20519,#20520,
#20521),.UNSPECIFIED.,.F.,.F.,(4,2,4),(0.0638119305867455,0.434740434623819,
0.895232561311264),.UNSPECIFIED.);
#692=B_SPLINE_CURVE_WITH_KNOTS('',3,(#20522,#20523,#20524,#20525,#20526,
#20527,#20528,#20529),.UNSPECIFIED.,.F.,.F.,(4,2,2,4),(0.0746811865707101,
0.397508022614198,0.744535688298082,1.0361955564677),.UNSPECIFIED.);
#693=B_SPLINE_CURVE_WITH_KNOTS('',3,(#20555,#20556,#20557,#20558,#20559,
#20560,#20561,#20562),.UNSPECIFIED.,.F.,.F.,(4,2,2,4),(0.0544345524991343,
0.140376841744944,0.193303927755901,0.233295962204409),.UNSPECIFIED.);
#694=B_SPLINE_CURVE_WITH_KNOTS('',3,(#20563,#20564,#20565,#20566,#20567,
#20568),.UNSPECIFIED.,.F.,.F.,(4,2,4),(0.0638119305867454,0.434740434623819,
0.895232561311264),.UNSPECIFIED.);
#695=B_SPLINE_CURVE_WITH_KNOTS('',3,(#20585,#20586,#20587,#20588,#20589,
#20590,#20591),.UNSPECIFIED.,.F.,.F.,(4,3,4),(0.,0.065379305383312,0.130355487793393),
 .UNSPECIFIED.);
#696=B_SPLINE_CURVE_WITH_KNOTS('',3,(#20594,#20595,#20596,#20597,#20598,
#20599,#20600,#20601),.UNSPECIFIED.,.F.,.F.,(4,2,2,4),(0.15440517711793,
0.438271814628381,0.790258491635719,1.12994605591353),.UNSPECIFIED.);
#697=B_SPLINE_CURVE_WITH_KNOTS('',3,(#20629,#20630,#20631,#20632,#20633,
#20634),.UNSPECIFIED.,.F.,.F.,(4,2,4),(0.,0.138460176943226,0.254919406847183),
 .UNSPECIFIED.);
#698=B_SPLINE_CURVE_WITH_KNOTS('',3,(#20635,#20636,#20637,#20638,#20639,
#20640),.UNSPECIFIED.,.F.,.F.,(4,2,4),(0.0638119305867456,0.434740434623819,
0.895232561311265),.UNSPECIFIED.);
#699=B_SPLINE_CURVE_WITH_KNOTS('',3,(#20641,#20642,#20643,#20644,#20645,
#20646,#20647,#20648),.UNSPECIFIED.,.F.,.F.,(4,2,2,4),(0.0746811865707119,
0.397508022614209,0.744535688298112,1.03619555646863),.UNSPECIFIED.);
#700=B_SPLINE_CURVE_WITH_KNOTS('',3,(#20674,#20675,#20676,#20677,#20678,
#20679,#20680,#20681),.UNSPECIFIED.,.F.,.F.,(4,2,2,4),(0.0544345524993946,
0.140376841745933,0.193303927757098,0.233295962203211),.UNSPECIFIED.);
#701=B_SPLINE_CURVE_WITH_KNOTS('',3,(#20682,#20683,#20684,#20685,#20686,
#20687),.UNSPECIFIED.,.F.,.F.,(4,2,4),(0.0638119305867456,0.434740434623819,
0.895232561311264),.UNSPECIFIED.);
#702=B_SPLINE_CURVE_WITH_KNOTS('',3,(#20704,#20705,#20706,#20707,#20708,
#20709,#20710),.UNSPECIFIED.,.F.,.F.,(4,3,4),(0.,0.0653793053833217,0.130355487793375),
 .UNSPECIFIED.);
#703=B_SPLINE_CURVE_WITH_KNOTS('',3,(#20713,#20714,#20715,#20716,#20717,
#20718,#20719,#20720),.UNSPECIFIED.,.F.,.F.,(4,2,2,4),(0.154405177117935,
0.4382718146284,0.790258491635752,1.12994605591357),.UNSPECIFIED.);
#704=B_SPLINE_CURVE_WITH_KNOTS('',3,(#20748,#20749,#20750,#20751,#20752,
#20753),.UNSPECIFIED.,.F.,.F.,(4,2,4),(0.,0.138460176944331,0.254919406857816),
 .UNSPECIFIED.);
#705=B_SPLINE_CURVE_WITH_KNOTS('',3,(#20754,#20755,#20756,#20757,#20758,
#20759),.UNSPECIFIED.,.F.,.F.,(4,2,4),(0.0638119305867456,0.434740434623819,
0.895232561311265),.UNSPECIFIED.);
#706=B_SPLINE_CURVE_WITH_KNOTS('',3,(#20760,#20761,#20762,#20763,#20764,
#20765,#20766,#20767),.UNSPECIFIED.,.F.,.F.,(4,2,2,4),(0.0746811865707107,
0.397508022614195,0.744535688298062,1.03619555646822),.UNSPECIFIED.);
#707=B_SPLINE_CURVE_WITH_KNOTS('',3,(#20793,#20794,#20795,#20796,#20797,
#20798,#20799,#20800),.UNSPECIFIED.,.F.,.F.,(4,2,2,4),(0.0544345524991419,
0.140376841744898,0.193303927757274,0.233295962207447),.UNSPECIFIED.);
#708=B_SPLINE_CURVE_WITH_KNOTS('',3,(#20801,#20802,#20803,#20804,#20805,
#20806),.UNSPECIFIED.,.F.,.F.,(4,2,4),(0.0638119305867456,0.434740434623819,
0.895232561311265),.UNSPECIFIED.);
#709=B_SPLINE_CURVE_WITH_KNOTS('',3,(#20823,#20824,#20825,#20826,#20827,
#20828,#20829),.UNSPECIFIED.,.F.,.F.,(4,3,4),(0.,0.065379305383224,0.13035548779319),
 .UNSPECIFIED.);
#710=B_SPLINE_CURVE_WITH_KNOTS('',3,(#20832,#20833,#20834,#20835,#20836,
#20837,#20838,#20839),.UNSPECIFIED.,.F.,.F.,(4,2,2,4),(0.154405177117924,
0.43827181462835,0.79025849163566,1.12994605591344),.UNSPECIFIED.);
#711=B_SPLINE_CURVE_WITH_KNOTS('',3,(#20866,#20867,#20868,#20869,#20870,
#20871),.UNSPECIFIED.,.F.,.F.,(4,2,4),(0.0638119305867455,0.434740434623819,
0.895232561311264),.UNSPECIFIED.);
#712=B_SPLINE_CURVE_WITH_KNOTS('',3,(#20872,#20873,#20874,#20875,#20876,
#20877,#20878,#20879),.UNSPECIFIED.,.F.,.F.,(4,2,2,4),(0.054434552499212,
0.140376841745297,0.193303927759282,0.233295962210278),.UNSPECIFIED.);
#713=B_SPLINE_CURVE_WITH_KNOTS('',3,(#20897,#20898,#20899,#20900,#20901,
#20902),.UNSPECIFIED.,.F.,.F.,(4,2,4),(0.0638119305867455,0.434740434623819,
0.895232561311264),.UNSPECIFIED.);
#714=B_SPLINE_CURVE_WITH_KNOTS('',3,(#20903,#20904,#20905,#20906,#20907,
#20908,#20909),.UNSPECIFIED.,.F.,.F.,(4,3,4),(0.,0.0653793053832804,0.130355487793316),
 .UNSPECIFIED.);
#715=B_SPLINE_CURVE_WITH_KNOTS('',3,(#20935,#20936,#20937,#20938,#20939,
#20940,#20941,#20942),.UNSPECIFIED.,.F.,.F.,(4,2,2,4),(0.0746811865707135,
0.397508022614223,0.744535688298131,1.05488349691753),.UNSPECIFIED.);
#716=B_SPLINE_CURVE_WITH_KNOTS('',3,(#20943,#20944,#20945,#20946,#20947,
#20948),.UNSPECIFIED.,.F.,.F.,(4,2,4),(0.,0.138460176944853,0.254919406867187),
 .UNSPECIFIED.);
#717=B_SPLINE_CURVE_WITH_KNOTS('',3,(#20974,#20975,#20976,#20977,#20978,
#20979),.UNSPECIFIED.,.F.,.F.,(4,2,4),(0.0638119305867456,0.434740434623819,
0.895232561311265),.UNSPECIFIED.);
#718=B_SPLINE_CURVE_WITH_KNOTS('',3,(#20981,#20982,#20983,#20984,#20985,
#20986,#20987,#20988),.UNSPECIFIED.,.F.,.F.,(4,2,2,4),(0.0544345524992891,
0.140376841745541,0.193303927759119,0.23329596220775),.UNSPECIFIED.);
#719=B_SPLINE_CURVE_WITH_KNOTS('',3,(#20989,#20990,#20991,#20992,#20993,
#20994,#20995,#20996),.UNSPECIFIED.,.F.,.F.,(4,2,2,4),(0.0774162478442987,
0.414979417786396,0.760655521250396,1.05194916247824),.UNSPECIFIED.);
#720=B_SPLINE_CURVE_WITH_KNOTS('',3,(#21014,#21015,#21016,#21017,#21018,
#21019),.UNSPECIFIED.,.F.,.F.,(4,2,4),(0.0638119305867456,0.434740434623819,
0.895232561311265),.UNSPECIFIED.);
#721=B_SPLINE_CURVE_WITH_KNOTS('',3,(#21020,#21021,#21022,#21023,#21024,
#21025,#21026),.UNSPECIFIED.,.F.,.F.,(4,3,4),(0.,0.0653793053833094,0.13035548779333),
 .UNSPECIFIED.);
#722=B_SPLINE_CURVE_WITH_KNOTS('',3,(#21051,#21052,#21053,#21054,#21055,
#21056),.UNSPECIFIED.,.F.,.F.,(4,2,4),(0.,0.13846017694525,0.254919406867388),
 .UNSPECIFIED.);
#723=B_SPLINE_CURVE_WITH_KNOTS('',3,(#21270,#21271,#21272,#21273,#21274,
#21275,#21276,#21277,#21278,#21279,#21280,#21281,#21282,#21283,#21284,#21285,
#21286,#21287,#21288,#21289,#21290,#21291,#21292,#21293,#21294,#21295,#21296,
#21297,#21298,#21299,#21300,#21301,#21302,#21303),.UNSPECIFIED.,.F.,.F.,
(4,3,3,3,3,3,3,3,3,3,3,4),(0.,0.0110116267986798,0.0198365927950272,0.0393688637311641,
0.0455583406049715,0.0493231568143408,0.0527005792502689,0.056916196494854,
0.0651768568763584,0.0788461297337949,0.0828398890027903,0.100882854089343),
 .UNSPECIFIED.);
#724=B_SPLINE_CURVE_WITH_KNOTS('',3,(#21305,#21306,#21307,#21308,#21309,
#21310,#21311,#21312,#21313,#21314,#21315,#21316,#21317,#21318),
 .UNSPECIFIED.,.F.,.F.,(4,1,1,1,1,1,1,1,1,2,4),(-0.889886066635509,-0.843971490026765,
-0.78979558357151,-0.749163653730069,-0.681443770661001,-0.654355817433373,
-0.627267864205746,-0.600179910978118,-0.573091957750491,-0.464740144839981,
-0.44137654239973),.UNSPECIFIED.);
#725=B_SPLINE_CURVE_WITH_KNOTS('',3,(#21320,#21321,#21322,#21323,#21324,
#21325,#21326,#21327,#21328,#21329,#21330,#21331),.UNSPECIFIED.,.F.,.F.,
(4,2,2,2,2,4),(0.,0.0358257028990328,0.131952299625094,0.148884451735932,
0.157379698574708,0.16223106694039),.UNSPECIFIED.);
#726=B_SPLINE_CURVE_WITH_KNOTS('',3,(#21333,#21334,#21335,#21336),
 .UNSPECIFIED.,.F.,.F.,(4,4),(0.549999999941368,1.),.UNSPECIFIED.);
#727=B_SPLINE_CURVE_WITH_KNOTS('',3,(#21338,#21339,#21340,#21341,#21342,
#21343,#21344,#21345,#21346,#21347,#21348,#21349,#21350,#21351,#21352,#21353),
 .UNSPECIFIED.,.F.,.F.,(4,1,2,1,1,1,1,1,1,1,1,1,4),(0.310721506882948,0.387730825861464,
0.464740144839981,0.573091957750491,0.600179910978118,0.627267864205746,
0.654355817433373,0.681443770661001,0.749163653730069,0.78979558357151,
0.843971490026765,0.89814739648202,0.929489890414014),.UNSPECIFIED.);
#728=B_SPLINE_CURVE_WITH_KNOTS('',3,(#21354,#21355,#21356,#21357,#21358,
#21359,#21360,#21361,#21362,#21363,#21364,#21365,#21366,#21367,#21368,#21369,
#21370),.UNSPECIFIED.,.F.,.F.,(4,1,1,1,1,1,1,1,1,1,1,1,1,1,4),(0.929489890414014,
0.952323302937276,1.00649920939253,1.06067511584779,1.11485102230304,1.1690269287583,
1.22320283521355,1.26383476505499,1.33155464812406,1.35864260135169,1.38573055457932,
1.41281850780694,1.43990646103457,1.49408236748983,1.54825827394508),
 .UNSPECIFIED.);
#729=B_SPLINE_CURVE_WITH_KNOTS('',3,(#21372,#21373,#21374,#21375,#21376,
#21377,#21378,#21379,#21380,#21381,#21382,#21383,#21384,#21385),
 .UNSPECIFIED.,.F.,.F.,(4,2,2,2,2,2,4),(0.16223106694039,0.163967550885131,
0.171180716857468,0.182777598096348,0.205784524866042,0.262730804446443,
0.324280670363194),.UNSPECIFIED.);
#730=B_SPLINE_CURVE_WITH_KNOTS('',3,(#21386,#21387,#21388,#21389,#21390,
#21391,#21392,#21393,#21394,#21395,#21396,#21397,#21398,#21399),
 .UNSPECIFIED.,.F.,.F.,(4,1,1,1,1,1,1,1,1,1,1,4),(-1.4176032384283,-1.41281850780694,
-1.38573055457932,-1.35864260135169,-1.33155464812406,-1.26383476505499,
-1.22320283521355,-1.1690269287583,-1.11485102230304,-1.06067511584779,
-1.00649920939253,-0.969093714192518),.UNSPECIFIED.);
#731=B_SPLINE_CURVE_WITH_KNOTS('',3,(#21406,#21407,#21408,#21409,#21410,
#21411,#21412,#21413,#21414,#21415,#21416,#21417),.UNSPECIFIED.,.F.,.F.,
(4,1,1,1,1,1,1,2,4),(-1.50954599357819,-1.43295998077967,-1.38938999215504,
-1.34582000353042,-1.25868002628116,-1.21511003765654,-1.17154004903191,
-1.08440007178266,-1.06103646934241),.UNSPECIFIED.);
#732=B_SPLINE_CURVE_WITH_KNOTS('',3,(#21423,#21424,#21425,#21426,#21427,
#21428,#21429,#21430,#21431,#21432,#21433,#21434,#21435,#21436),
 .UNSPECIFIED.,.F.,.F.,(4,1,1,1,2,2,1,1,1,4),(-2.03726316537097,-2.03275764211163,
-2.01344899085789,-1.93621438584296,-1.85897978082803,-1.78151988977668,
-1.71616490683974,-1.69437991252743,-1.60723993527817,-1.58875364113519),
 .UNSPECIFIED.);
#733=B_SPLINE_CURVE_WITH_KNOTS('',3,(#21442,#21443,#21444,#21445,#21446,
#21447,#21448,#21449,#21450,#21451),.UNSPECIFIED.,.F.,.F.,(4,2,2,2,4),(0.,
0.0782721603764034,0.156544320752807,0.234729089704077,0.312913858655347),
 .UNSPECIFIED.);
#734=B_SPLINE_CURVE_WITH_KNOTS('',3,(#21452,#21453,#21454,#21455,#21456,
#21457,#21458,#21459,#21460,#21461,#21462,#21463,#21464,#21465,#21466,#21467,
#21468,#21469,#21470,#21471,#21472,#21473,#21474,#21475,#21476,#21477),
 .UNSPECIFIED.,.F.,.F.,(4,2,2,2,2,2,2,2,2,2,2,2,4),(0.312913858655347,0.391098627606618,
0.469283396557888,0.547555556934292,0.625827717310695,0.704099877687098,
0.782372038063502,0.860556807014772,0.938741575966043,1.01692634491731,
1.09511111386858,1.17338327424499,1.25165543462139),.UNSPECIFIED.);
#735=B_SPLINE_CURVE_WITH_KNOTS('',3,(#21590,#21591,#21592,#21593,#21594,
#21595,#21596,#21597,#21598,#21599,#21600,#21601,#21602,#21603,#21604,#21605,
#21606,#21607,#21608,#21609,#21610,#21611,#21612,#21613,#21614,#21615,#21616,
#21617,#21618,#21619,#21620,#21621,#21622,#21623,#21624,#21625,#21626),
 .UNSPECIFIED.,.F.,.F.,(4,3,3,3,3,3,3,3,3,3,3,3,4),(0.,0.0140126898858465,
0.0198365927950119,0.0393688637311589,0.0455583406050571,0.0493231568139791,
0.0527005792494364,0.0569161964938546,0.0651768568751002,0.0683276956644967,
0.0828398890011837,0.0964479725722503,0.100882854087323),.UNSPECIFIED.);
#736=B_SPLINE_CURVE_WITH_KNOTS('',3,(#21628,#21629,#21630,#21631,#21632,
#21633,#21634,#21635,#21636,#21637,#21638,#21639),.UNSPECIFIED.,.F.,.F.,
(4,2,2,2,2,4),(0.,0.0358257028990433,0.131952299625135,0.148884451735976,
0.157379698574799,0.162231066940522),.UNSPECIFIED.);
#737=B_SPLINE_CURVE_WITH_KNOTS('',3,(#21641,#21642,#21643,#21644),
 .UNSPECIFIED.,.F.,.F.,(4,4),(0.549999999941368,1.),.UNSPECIFIED.);
#738=B_SPLINE_CURVE_WITH_KNOTS('',3,(#21646,#21647,#21648,#21649,#21650,
#21651,#21652,#21653,#21654,#21655,#21656,#21657,#21658,#21659),
 .UNSPECIFIED.,.F.,.F.,(4,1,2,1,1,1,1,1,1,1,4),(0.930381433825624,1.00739075280414,
1.08440007178266,1.17154004903191,1.21511003765654,1.25868002628116,1.34582000353042,
1.38938999215504,1.43295998077967,1.52009995802892,1.54914981735669),
 .UNSPECIFIED.);
#739=B_SPLINE_CURVE_WITH_KNOTS('',3,(#21660,#21661,#21662,#21663,#21664,
#21665,#21666,#21667,#21668,#21669,#21670,#21671,#21672,#21673,#21674,#21675,
#21676,#21677),.UNSPECIFIED.,.F.,.F.,(4,1,1,1,1,1,2,2,1,1,1,1,1,4),(1.54914981735669,
1.56366994665355,1.58545494096586,1.60723993527817,1.69437991252743,1.71616490683974,
1.78151988977668,1.85897978082803,1.93621438584296,2.01344899085789,2.03275764211163,
2.05206629336536,2.09068359587282,2.16791820088776),.UNSPECIFIED.);
#740=B_SPLINE_CURVE_WITH_KNOTS('',3,(#21678,#21679,#21680,#21681,#21682,
#21683,#21684,#21685,#21686,#21687,#21688,#21689,#21690,#21691),
 .UNSPECIFIED.,.F.,.F.,(4,2,2,2,2,2,4),(0.162231066940522,0.163967550885278,
0.171180716857662,0.182777598096494,0.205784524865831,0.262730804445425,
0.324280670361326),.UNSPECIFIED.);
#741=B_SPLINE_CURVE_WITH_KNOTS('',3,(#21695,#21696,#21697,#21698,#21699,
#21700,#21701,#21702,#21703,#21704,#21705,#21706,#21707,#21708,#21709,#21710,
#21711,#21712,#21713,#21714,#21715,#21716,#21717,#21718,#21719,#21720),
 .UNSPECIFIED.,.F.,.F.,(4,2,2,2,2,2,2,2,2,2,2,2,4),(0.,0.0782721603764034,
0.156544320752807,0.234729089704077,0.312913858655348,0.391098627606618,
0.469283396557888,0.547555556934292,0.625827717310695,0.704099877687099,
0.782372038063502,0.860556807014772,0.938741575966043),.UNSPECIFIED.);
#742=B_SPLINE_CURVE_WITH_KNOTS('',3,(#21721,#21722,#21723,#21724,#21725,
#21726,#21727,#21728,#21729,#21730),.UNSPECIFIED.,.F.,.F.,(4,2,2,2,4),(0.938741575966043,
1.01692634491731,1.09511111386858,1.17338327424499,1.25165543462139),
 .UNSPECIFIED.);
#743=B_SPLINE_CURVE_WITH_KNOTS('',3,(#21762,#21763,#21764,#21765,#21766,
#21767),.UNSPECIFIED.,.F.,.F.,(4,2,4),(0.,0.138207529108851,0.257151380447634),
 .UNSPECIFIED.);
#744=B_SPLINE_CURVE_WITH_KNOTS('',3,(#21769,#21770,#21771,#21772,#21773,
#21774),.UNSPECIFIED.,.F.,.F.,(4,2,4),(0.0638119305867455,0.434740434623819,
0.895232561311264),.UNSPECIFIED.);
#745=B_SPLINE_CURVE_WITH_KNOTS('',3,(#21776,#21777,#21778,#21779,#21780,
#21781,#21782,#21783),.UNSPECIFIED.,.F.,.F.,(4,2,2,4),(0.0650199495982317,
0.170565165416136,0.226763969189742,0.268056752438448),.UNSPECIFIED.);
#746=B_SPLINE_CURVE_WITH_KNOTS('',3,(#21784,#21785,#21786,#21787,#21788,
#21789,#21790,#21791),.UNSPECIFIED.,.F.,.F.,(4,2,2,4),(0.0747583116411992,
0.415738779002342,0.772551101530307,1.04863108973719),.UNSPECIFIED.);
#747=B_SPLINE_CURVE_WITH_KNOTS('',3,(#21818,#21819,#21820,#21821,#21822,
#21823,#21824,#21825),.UNSPECIFIED.,.F.,.F.,(4,2,2,4),(0.0535030672285043,
0.137418922872643,0.199655718694958,0.252976612949483),.UNSPECIFIED.);
#748=B_SPLINE_CURVE_WITH_KNOTS('',3,(#21827,#21828,#21829,#21830,#21831,
#21832,#21833,#21834),.UNSPECIFIED.,.F.,.F.,(4,2,2,4),(0.11834343350373,
0.512336851961602,0.931707568041671,1.28239107793921),.UNSPECIFIED.);
#749=B_SPLINE_CURVE_WITH_KNOTS('',3,(#21836,#21837,#21838,#21839,#21840,
#21841),.UNSPECIFIED.,.F.,.F.,(4,2,4),(0.,0.208309927739493,0.384486154932789),
 .UNSPECIFIED.);
#750=B_SPLINE_CURVE_WITH_KNOTS('',3,(#21842,#21843,#21844,#21845,#21846,
#21847),.UNSPECIFIED.,.F.,.F.,(4,2,4),(0.0638119305867455,0.434740434623819,
0.895232561311264),.UNSPECIFIED.);
#751=B_SPLINE_CURVE_WITH_KNOTS('',3,(#21864,#21865,#21866,#21867,#21868,
#21869,#21870),.UNSPECIFIED.,.F.,.F.,(4,3,4),(0.,0.064975255706308,0.13035708562273),
 .UNSPECIFIED.);
#752=B_SPLINE_CURVE_WITH_KNOTS('',3,(#21871,#21872,#21873,#21874,#21875,
#21876,#21877),.UNSPECIFIED.,.F.,.F.,(4,3,4),(0.,0.0981730480407086,0.191890424805344),
 .UNSPECIFIED.);
#753=B_SPLINE_CURVE_WITH_KNOTS('',3,(#21884,#21885,#21886,#21887),
 .UNSPECIFIED.,.F.,.F.,(4,4),(0.331995637616086,0.384486154832915),
 .UNSPECIFIED.);
#754=B_SPLINE_CURVE_WITH_KNOTS('',3,(#21891,#21892,#21893,#21894,#21895,
#21896,#21897,#21898),.UNSPECIFIED.,.F.,.F.,(4,2,2,4),(0.0542087124698116,
0.203323725897707,0.32378750142016,0.520894956620335),.UNSPECIFIED.);
#755=B_SPLINE_CURVE_WITH_KNOTS('',3,(#21900,#21901,#21902,#21903,#21904,
#21905,#21906),.UNSPECIFIED.,.F.,.F.,(4,3,4),(0.,0.0981730480406908,0.191890424805207),
 .UNSPECIFIED.);
#756=B_SPLINE_CURVE_WITH_KNOTS('',3,(#21908,#21909,#21910,#21911,#21912,
#21913),.UNSPECIFIED.,.F.,.F.,(4,2,4),(0.,0.208309927750236,0.384486155029173),
 .UNSPECIFIED.);
#757=B_SPLINE_CURVE_WITH_KNOTS('',3,(#21917,#21918,#21919,#21920,#21921,
#21922,#21923,#21924),.UNSPECIFIED.,.F.,.F.,(4,2,2,4),(0.0650199496529384,
0.170565165647366,0.226763969524849,0.268056752853526),.UNSPECIFIED.);
#758=B_SPLINE_CURVE_WITH_KNOTS('',3,(#21926,#21927,#21928,#21929,#21930,
#21931,#21932),.UNSPECIFIED.,.F.,.F.,(4,3,4),(0.,0.0981730480406766,0.191890424805293),
 .UNSPECIFIED.);
#759=B_SPLINE_CURVE_WITH_KNOTS('',3,(#21934,#21935,#21936,#21937,#21938,
#21939),.UNSPECIFIED.,.F.,.F.,(4,2,4),(0.,0.208309927746205,0.38448615499989),
 .UNSPECIFIED.);
#760=B_SPLINE_CURVE_WITH_KNOTS('',3,(#21943,#21944,#21945,#21946,#21947,
#21948,#21949,#21950),.UNSPECIFIED.,.F.,.F.,(4,2,2,4),(0.0650199495839021,
0.170565165355256,0.226763969103251,0.268056752329737),.UNSPECIFIED.);
#761=B_SPLINE_CURVE_WITH_KNOTS('',3,(#21952,#21953,#21954,#21955,#21956,
#21957,#21958),.UNSPECIFIED.,.F.,.F.,(4,3,4),(0.,0.0981730480407384,0.191890424805265),
 .UNSPECIFIED.);
#762=B_SPLINE_CURVE_WITH_KNOTS('',3,(#21960,#21961,#21962,#21963,#21964,
#21965),.UNSPECIFIED.,.F.,.F.,(4,2,4),(0.,0.208309927742208,0.384486154882329),
 .UNSPECIFIED.);
#763=B_SPLINE_CURVE_WITH_KNOTS('',3,(#21969,#21970,#21971,#21972,#21973,
#21974,#21975,#21976),.UNSPECIFIED.,.F.,.F.,(4,2,2,4),(0.0650199495860717,
0.170565165364572,0.226763969117006,0.26805675235156),.UNSPECIFIED.);
#764=B_SPLINE_CURVE_WITH_KNOTS('',3,(#21978,#21979,#21980,#21981,#21982,
#21983,#21984),.UNSPECIFIED.,.F.,.F.,(4,3,4),(0.,0.098173048040732,0.191890424805364),
 .UNSPECIFIED.);
#765=B_SPLINE_CURVE_WITH_KNOTS('',3,(#21986,#21987,#21988,#21989,#21990,
#21991),.UNSPECIFIED.,.F.,.F.,(4,2,4),(0.,0.208309927745551,0.38448615497379),
 .UNSPECIFIED.);
#766=B_SPLINE_CURVE_WITH_KNOTS('',3,(#21995,#21996,#21997,#21998,#21999,
#22000,#22001,#22002),.UNSPECIFIED.,.F.,.F.,(4,2,2,4),(0.0650199495587532,
0.170565165249151,0.226763968946711,0.268056752139196),.UNSPECIFIED.);
#767=B_SPLINE_CURVE_WITH_KNOTS('',3,(#22004,#22005,#22006,#22007,#22008,
#22009,#22010),.UNSPECIFIED.,.F.,.F.,(4,3,4),(0.,0.098173048040845,0.191890424805652),
 .UNSPECIFIED.);
#768=B_SPLINE_CURVE_WITH_KNOTS('',3,(#22012,#22013,#22014,#22015,#22016,
#22017),.UNSPECIFIED.,.F.,.F.,(4,2,4),(0.,0.208309927731817,0.384486154823123),
 .UNSPECIFIED.);
#769=B_SPLINE_CURVE_WITH_KNOTS('',3,(#22021,#22022,#22023,#22024,#22025,
#22026,#22027,#22028),.UNSPECIFIED.,.F.,.F.,(4,2,2,4),(0.054208712440581,
0.203323725621083,0.32378750087977,0.520894955605601),.UNSPECIFIED.);
#770=B_SPLINE_CURVE_WITH_KNOTS('',3,(#22030,#22031,#22032,#22033,#22034,
#22035,#22036),.UNSPECIFIED.,.F.,.F.,(4,3,4),(0.,0.0981730480406625,0.19189042480521),
 .UNSPECIFIED.);
#771=B_SPLINE_CURVE_WITH_KNOTS('',3,(#22038,#22039,#22040,#22041,#22042,
#22043),.UNSPECIFIED.,.F.,.F.,(4,2,4),(0.,0.208309927743994,0.384486154966103),
 .UNSPECIFIED.);
#772=B_SPLINE_CURVE_WITH_KNOTS('',3,(#22047,#22048,#22049,#22050,#22051,
#22052,#22053,#22054),.UNSPECIFIED.,.F.,.F.,(4,2,2,4),(0.0650199496372336,
0.170565165580817,0.226763969430302,0.268056752734932),.UNSPECIFIED.);
#773=B_SPLINE_CURVE_WITH_KNOTS('',3,(#22056,#22057,#22058,#22059,#22060,
#22061,#22062),.UNSPECIFIED.,.F.,.F.,(4,3,4),(0.,0.0981730480407077,0.191890424805375),
 .UNSPECIFIED.);
#774=B_SPLINE_CURVE_WITH_KNOTS('',3,(#22064,#22065,#22066,#22067,#22068,
#22069),.UNSPECIFIED.,.F.,.F.,(4,2,4),(0.,0.20830992773469,0.384486154871887),
 .UNSPECIFIED.);
#775=B_SPLINE_CURVE_WITH_KNOTS('',3,(#22073,#22074,#22075,#22076,#22077,
#22078,#22079,#22080),.UNSPECIFIED.,.F.,.F.,(4,2,2,4),(0.0650199495866873,
0.170565165367095,0.226763969117418,0.268056752346729),.UNSPECIFIED.);
#776=B_SPLINE_CURVE_WITH_KNOTS('',3,(#22082,#22083,#22084,#22085,#22086,
#22087,#22088),.UNSPECIFIED.,.F.,.F.,(4,3,4),(0.,0.0981730480407126,0.191890424805348),
 .UNSPECIFIED.);
#777=B_SPLINE_CURVE_WITH_KNOTS('',3,(#22090,#22091,#22092,#22093,#22094,
#22095),.UNSPECIFIED.,.F.,.F.,(4,2,4),(0.,0.208309927751894,0.384486154960954),
 .UNSPECIFIED.);
#778=B_SPLINE_CURVE_WITH_KNOTS('',3,(#22099,#22100,#22101,#22102,#22103,
#22104,#22105,#22106),.UNSPECIFIED.,.F.,.F.,(4,2,2,4),(0.0650199495073989,
0.170565165032043,0.226763968637804,0.268056751759602),.UNSPECIFIED.);
#779=B_SPLINE_CURVE_WITH_KNOTS('',3,(#22108,#22109,#22110,#22111,#22112,
#22113,#22114),.UNSPECIFIED.,.F.,.F.,(4,3,4),(0.,0.0981730480406239,0.191890424805078),
 .UNSPECIFIED.);
#780=B_SPLINE_CURVE_WITH_KNOTS('',3,(#22116,#22117,#22118,#22119,#22120,
#22121),.UNSPECIFIED.,.F.,.F.,(4,2,4),(0.,0.20830992772829,0.384486154840441),
 .UNSPECIFIED.);
#781=B_SPLINE_CURVE_WITH_KNOTS('',3,(#22126,#22127,#22128,#22129,#22130,
#22131,#22132,#22133),.UNSPECIFIED.,.F.,.F.,(4,2,2,4),(0.0542611019730315,
0.202920016768632,0.323128184799993,0.520330951478027),.UNSPECIFIED.);
#782=B_SPLINE_CURVE_WITH_KNOTS('',3,(#22135,#22136,#22137,#22138,#22139,
#22140,#22141),.UNSPECIFIED.,.F.,.F.,(4,3,4),(0.,0.0981730480406862,0.19189042480528),
 .UNSPECIFIED.);
#783=B_SPLINE_CURVE_WITH_KNOTS('',3,(#22143,#22144,#22145,#22146,#22147,
#22148),.UNSPECIFIED.,.F.,.F.,(4,2,4),(0.,0.208309927742973,0.38448615495736),
 .UNSPECIFIED.);
#784=B_SPLINE_CURVE_WITH_KNOTS('',3,(#22152,#22153,#22154,#22155,#22156,
#22157,#22158,#22159),.UNSPECIFIED.,.F.,.F.,(4,2,2,4),(0.0650199495256298,
0.170565165109065,0.226763968747303,0.268056751893518),.UNSPECIFIED.);
#785=B_SPLINE_CURVE_WITH_KNOTS('',3,(#22161,#22162,#22163,#22164,#22165,
#22166,#22167),.UNSPECIFIED.,.F.,.F.,(4,3,4),(0.,0.0981730480407225,0.191890424805355),
 .UNSPECIFIED.);
#786=B_SPLINE_CURVE_WITH_KNOTS('',3,(#22169,#22170,#22171,#22172,#22173,
#22174),.UNSPECIFIED.,.F.,.F.,(4,2,4),(0.,0.208309927727119,0.384486154806359),
 .UNSPECIFIED.);
#787=B_SPLINE_CURVE_WITH_KNOTS('',3,(#22178,#22179,#22180,#22181,#22182,
#22183,#22184,#22185),.UNSPECIFIED.,.F.,.F.,(4,2,2,4),(0.0650199496379536,
0.170565165583986,0.22676396943225,0.26805675273395),.UNSPECIFIED.);
#788=B_SPLINE_CURVE_WITH_KNOTS('',3,(#22187,#22188,#22189,#22190,#22191,
#22192,#22193),.UNSPECIFIED.,.F.,.F.,(4,3,4),(0.,0.0981730480407346,0.191890424805321),
 .UNSPECIFIED.);
#789=B_SPLINE_CURVE_WITH_KNOTS('',3,(#22195,#22196,#22197,#22198,#22199,
#22200),.UNSPECIFIED.,.F.,.F.,(4,2,4),(0.,0.208309927739911,0.384486154953153),
 .UNSPECIFIED.);
#790=B_SPLINE_CURVE_WITH_KNOTS('',3,(#22204,#22205,#22206,#22207,#22208,
#22209,#22210,#22211),.UNSPECIFIED.,.F.,.F.,(4,2,2,4),(0.0650199495498999,
0.170565165211631,0.226763968890252,0.268056752070099),.UNSPECIFIED.);
#791=B_SPLINE_CURVE_WITH_KNOTS('',3,(#22213,#22214,#22215,#22216,#22217,
#22218,#22219),.UNSPECIFIED.,.F.,.F.,(4,3,4),(0.,0.098173048040742,0.191890424805327),
 .UNSPECIFIED.);
#792=B_SPLINE_CURVE_WITH_KNOTS('',3,(#22221,#22222,#22223,#22224,#22225,
#22226),.UNSPECIFIED.,.F.,.F.,(4,2,4),(0.,0.208309927725018,0.384486154743549),
 .UNSPECIFIED.);
#793=B_SPLINE_CURVE_WITH_KNOTS('',3,(#22230,#22231,#22232,#22233,#22234,
#22235,#22236,#22237),.UNSPECIFIED.,.F.,.F.,(4,2,2,4),(0.0650199494135083,
0.170565164635192,0.22676396805462,0.268056751043425),.UNSPECIFIED.);
#794=B_SPLINE_CURVE_WITH_KNOTS('',3,(#22239,#22240,#22241,#22242,#22243,
#22244,#22245),.UNSPECIFIED.,.F.,.F.,(4,3,4),(0.,0.098173048040714,0.191890424805356),
 .UNSPECIFIED.);
#795=B_SPLINE_CURVE_WITH_KNOTS('',3,(#22247,#22248,#22249,#22250,#22251,
#22252),.UNSPECIFIED.,.F.,.F.,(4,2,4),(0.,0.208309927737883,0.384486154890492),
 .UNSPECIFIED.);
#796=B_SPLINE_CURVE_WITH_KNOTS('',3,(#22256,#22257,#22258,#22259,#22260,
#22261,#22262,#22263),.UNSPECIFIED.,.F.,.F.,(4,2,2,4),(0.0542087124218259,
0.203323725443623,0.323787500531832,0.520894954944429),.UNSPECIFIED.);
#797=B_SPLINE_CURVE_WITH_KNOTS('',3,(#22265,#22266,#22267,#22268,#22269,
#22270,#22271),.UNSPECIFIED.,.F.,.F.,(4,3,4),(0.,0.098173048040669,0.191890424805223),
 .UNSPECIFIED.);
#798=B_SPLINE_CURVE_WITH_KNOTS('',3,(#22273,#22274,#22275,#22276,#22277,
#22278),.UNSPECIFIED.,.F.,.F.,(4,2,4),(0.,0.208309927750018,0.384486155023449),
 .UNSPECIFIED.);
#799=B_SPLINE_CURVE_WITH_KNOTS('',3,(#22282,#22283,#22284,#22285,#22286,
#22287,#22288,#22289),.UNSPECIFIED.,.F.,.F.,(4,2,2,4),(0.0650199496369929,
0.170565165579854,0.226763969431761,0.268056752734831),.UNSPECIFIED.);
#800=B_SPLINE_CURVE_WITH_KNOTS('',3,(#22291,#22292,#22293,#22294,#22295,
#22296,#22297),.UNSPECIFIED.,.F.,.F.,(4,3,4),(0.,0.098173048040829,0.191890424805588),
 .UNSPECIFIED.);
#801=B_SPLINE_CURVE_WITH_KNOTS('',3,(#22299,#22300,#22301,#22302,#22303,
#22304),.UNSPECIFIED.,.F.,.F.,(4,2,4),(0.,0.208309927736197,0.384486154842889),
 .UNSPECIFIED.);
#802=B_SPLINE_CURVE_WITH_KNOTS('',3,(#22308,#22309,#22310,#22311,#22312,
#22313,#22314,#22315),.UNSPECIFIED.,.F.,.F.,(4,2,2,4),(0.0650199495839219,
0.170565165355339,0.226763969103371,0.268056752329883),.UNSPECIFIED.);
#803=B_SPLINE_CURVE_WITH_KNOTS('',3,(#22317,#22318,#22319,#22320,#22321,
#22322,#22323),.UNSPECIFIED.,.F.,.F.,(4,3,4),(0.,0.0981730480406805,0.191890424805183),
 .UNSPECIFIED.);
#804=B_SPLINE_CURVE_WITH_KNOTS('',3,(#22325,#22326,#22327,#22328,#22329,
#22330),.UNSPECIFIED.,.F.,.F.,(4,2,4),(0.,0.208309927742222,0.384486154882313),
 .UNSPECIFIED.);
#805=B_SPLINE_CURVE_WITH_KNOTS('',3,(#22334,#22335,#22336,#22337,#22338,
#22339,#22340,#22341),.UNSPECIFIED.,.F.,.F.,(4,2,2,4),(0.0650199495861818,
0.170565165365035,0.226763969117688,0.268056752352361),.UNSPECIFIED.);
#806=B_SPLINE_CURVE_WITH_KNOTS('',3,(#22343,#22344,#22345,#22346,#22347,
#22348,#22349),.UNSPECIFIED.,.F.,.F.,(4,3,4),(0.,0.0981730480406793,0.191890424805241),
 .UNSPECIFIED.);
#807=B_SPLINE_CURVE_WITH_KNOTS('',3,(#22351,#22352,#22353,#22354,#22355,
#22356),.UNSPECIFIED.,.F.,.F.,(4,2,4),(0.,0.208309927745549,0.384486154973776),
 .UNSPECIFIED.);
#808=B_SPLINE_CURVE_WITH_KNOTS('',3,(#22360,#22361,#22362,#22363,#22364,
#22365,#22366,#22367),.UNSPECIFIED.,.F.,.F.,(4,2,2,4),(0.0650199495195806,
0.1705651650837,0.226763968706434,0.268056751843866),.UNSPECIFIED.);
#809=B_SPLINE_CURVE_WITH_KNOTS('',3,(#22369,#22370,#22371,#22372,#22373,
#22374,#22375),.UNSPECIFIED.,.F.,.F.,(4,3,4),(0.,0.0981730480406788,0.191890424805225),
 .UNSPECIFIED.);
#810=B_SPLINE_CURVE_WITH_KNOTS('',3,(#22376,#22377,#22378,#22379,#22380,
#22381),.UNSPECIFIED.,.F.,.F.,(4,2,4),(0.,0.208309927731304,0.331995637616086),
 .UNSPECIFIED.);
#811=B_SPLINE_CURVE_WITH_KNOTS('',3,(#22385,#22386,#22387,#22388,#22389,
#22390,#22391,#22392),.UNSPECIFIED.,.F.,.F.,(4,2,2,4),(0.0747583116412021,
0.415738779002311,0.753026862713569,1.0479673638265),.UNSPECIFIED.);
#812=B_SPLINE_CURVE_WITH_KNOTS('',3,(#22395,#22396,#22397,#22398,#22399,
#22400,#22401,#22402),.UNSPECIFIED.,.F.,.F.,(4,2,2,4),(0.154059232628148,
0.534434525764867,0.968745967316882,1.33329265533026),.UNSPECIFIED.);
#813=B_SPLINE_CURVE_WITH_KNOTS('',3,(#22430,#22431,#22432,#22433,#22434,
#22435),.UNSPECIFIED.,.F.,.F.,(4,2,4),(0.,0.138207529109353,0.25715138045422),
 .UNSPECIFIED.);
#814=B_SPLINE_CURVE_WITH_KNOTS('',3,(#22436,#22437,#22438,#22439,#22440,
#22441),.UNSPECIFIED.,.F.,.F.,(4,2,4),(0.0638119305867454,0.434740434623819,
0.895232561311264),.UNSPECIFIED.);
#815=B_SPLINE_CURVE_WITH_KNOTS('',3,(#22442,#22443,#22444,#22445,#22446,
#22447,#22448,#22449),.UNSPECIFIED.,.F.,.F.,(4,2,2,4),(0.0747583116411993,
0.415738779002422,0.772551101530389,1.0486310897372),.UNSPECIFIED.);
#816=B_SPLINE_CURVE_WITH_KNOTS('',3,(#22475,#22476,#22477,#22478,#22479,
#22480,#22481,#22482),.UNSPECIFIED.,.F.,.F.,(4,2,2,4),(0.053503067227966,
0.137418922870269,0.199655718696157,0.252976612954111),.UNSPECIFIED.);
#817=B_SPLINE_CURVE_WITH_KNOTS('',3,(#22483,#22484,#22485,#22486,#22487,
#22488),.UNSPECIFIED.,.F.,.F.,(4,2,4),(0.0638119305867453,0.434740434623819,
0.895232561311263),.UNSPECIFIED.);
#818=B_SPLINE_CURVE_WITH_KNOTS('',3,(#22505,#22506,#22507,#22508,#22509,
#22510,#22511),.UNSPECIFIED.,.F.,.F.,(4,3,4),(0.,0.0649752557063318,0.130357085622803),
 .UNSPECIFIED.);
#819=B_SPLINE_CURVE_WITH_KNOTS('',3,(#22514,#22515,#22516,#22517,#22518,
#22519,#22520,#22521),.UNSPECIFIED.,.F.,.F.,(4,2,2,4),(0.154059232628334,
0.534434525767114,0.968745967322665,1.33329265533901),.UNSPECIFIED.);
#820=B_SPLINE_CURVE_WITH_KNOTS('',3,(#22549,#22550,#22551,#22552,#22553,
#22554),.UNSPECIFIED.,.F.,.F.,(4,2,4),(0.,0.138207529109416,0.257151380444098),
 .UNSPECIFIED.);
#821=B_SPLINE_CURVE_WITH_KNOTS('',3,(#22555,#22556,#22557,#22558,#22559,
#22560),.UNSPECIFIED.,.F.,.F.,(4,2,4),(0.0638119305867455,0.434740434623819,
0.895232561311264),.UNSPECIFIED.);
#822=B_SPLINE_CURVE_WITH_KNOTS('',3,(#22561,#22562,#22563,#22564,#22565,
#22566,#22567,#22568),.UNSPECIFIED.,.F.,.F.,(4,2,2,4),(0.0747583116412007,
0.41573877900245,0.772551101530441,1.04863108973726),.UNSPECIFIED.);
#823=B_SPLINE_CURVE_WITH_KNOTS('',3,(#22594,#22595,#22596,#22597,#22598,
#22599,#22600,#22601),.UNSPECIFIED.,.F.,.F.,(4,2,2,4),(0.0535030672291814,
0.137418922876081,0.19965571870634,0.252976612971294),.UNSPECIFIED.);
#824=B_SPLINE_CURVE_WITH_KNOTS('',3,(#22602,#22603,#22604,#22605,#22606,
#22607),.UNSPECIFIED.,.F.,.F.,(4,2,4),(0.0638119305867455,0.434740434623819,
0.895232561311264),.UNSPECIFIED.);
#825=B_SPLINE_CURVE_WITH_KNOTS('',3,(#22624,#22625,#22626,#22627,#22628,
#22629,#22630),.UNSPECIFIED.,.F.,.F.,(4,3,4),(0.,0.0649752557062639,0.130357085622636),
 .UNSPECIFIED.);
#826=B_SPLINE_CURVE_WITH_KNOTS('',3,(#22633,#22634,#22635,#22636,#22637,
#22638,#22639,#22640),.UNSPECIFIED.,.F.,.F.,(4,2,2,4),(0.154059232628307,
0.534434525766854,0.968745967321853,1.33329265533773),.UNSPECIFIED.);
#827=B_SPLINE_CURVE_WITH_KNOTS('',3,(#22668,#22669,#22670,#22671,#22672,
#22673),.UNSPECIFIED.,.F.,.F.,(4,2,4),(0.,0.138207529110581,0.257151380456836),
 .UNSPECIFIED.);
#828=B_SPLINE_CURVE_WITH_KNOTS('',3,(#22674,#22675,#22676,#22677,#22678,
#22679),.UNSPECIFIED.,.F.,.F.,(4,2,4),(0.0638119305867455,0.434740434623819,
0.895232561311264),.UNSPECIFIED.);
#829=B_SPLINE_CURVE_WITH_KNOTS('',3,(#22680,#22681,#22682,#22683,#22684,
#22685,#22686,#22687),.UNSPECIFIED.,.F.,.F.,(4,2,2,4),(0.0747583116412006,
0.415738779002382,0.772551101530378,1.04863108973727),.UNSPECIFIED.);
#830=B_SPLINE_CURVE_WITH_KNOTS('',3,(#22713,#22714,#22715,#22716,#22717,
#22718,#22719,#22720),.UNSPECIFIED.,.F.,.F.,(4,2,2,4),(0.0535030672284625,
0.137418922872139,0.199655718694633,0.252976612947559),.UNSPECIFIED.);
#831=B_SPLINE_CURVE_WITH_KNOTS('',3,(#22721,#22722,#22723,#22724,#22725,
#22726),.UNSPECIFIED.,.F.,.F.,(4,2,4),(0.0638119305867455,0.434740434623819,
0.895232561311264),.UNSPECIFIED.);
#832=B_SPLINE_CURVE_WITH_KNOTS('',3,(#22743,#22744,#22745,#22746,#22747,
#22748,#22749),.UNSPECIFIED.,.F.,.F.,(4,3,4),(0.,0.0649752557062745,0.130357085622644),
 .UNSPECIFIED.);
#833=B_SPLINE_CURVE_WITH_KNOTS('',3,(#22752,#22753,#22754,#22755,#22756,
#22757,#22758,#22759),.UNSPECIFIED.,.F.,.F.,(4,2,2,4),(0.154059232628089,
0.534434525764075,0.968745967315031,1.33329265532752),.UNSPECIFIED.);
#834=B_SPLINE_CURVE_WITH_KNOTS('',3,(#22787,#22788,#22789,#22790,#22791,
#22792),.UNSPECIFIED.,.F.,.F.,(4,2,4),(0.,0.138207529113509,0.257151380470495),
 .UNSPECIFIED.);
#835=B_SPLINE_CURVE_WITH_KNOTS('',3,(#22793,#22794,#22795,#22796,#22797,
#22798),.UNSPECIFIED.,.F.,.F.,(4,2,4),(0.0638119305867455,0.434740434623819,
0.895232561311264),.UNSPECIFIED.);
#836=B_SPLINE_CURVE_WITH_KNOTS('',3,(#22799,#22800,#22801,#22802,#22803,
#22804,#22805,#22806),.UNSPECIFIED.,.F.,.F.,(4,2,2,4),(0.0747583116412008,
0.415738779002339,0.752886816639909,1.04796308482473),.UNSPECIFIED.);
#837=B_SPLINE_CURVE_WITH_KNOTS('',3,(#22832,#22833,#22834,#22835,#22836,
#22837,#22838,#22839),.UNSPECIFIED.,.F.,.F.,(4,2,2,4),(0.0535030672285657,
0.137418922872968,0.199655718696181,0.252976612951919),.UNSPECIFIED.);
#838=B_SPLINE_CURVE_WITH_KNOTS('',3,(#22840,#22841,#22842,#22843,#22844,
#22845),.UNSPECIFIED.,.F.,.F.,(4,2,4),(0.0638119305867455,0.434740434623819,
0.895232561311264),.UNSPECIFIED.);
#839=B_SPLINE_CURVE_WITH_KNOTS('',3,(#22862,#22863,#22864,#22865,#22866,
#22867,#22868),.UNSPECIFIED.,.F.,.F.,(4,3,4),(0.,0.0649752557062603,0.130357085622615),
 .UNSPECIFIED.);
#840=B_SPLINE_CURVE_WITH_KNOTS('',3,(#22871,#22872,#22873,#22874,#22875,
#22876,#22877,#22878),.UNSPECIFIED.,.F.,.F.,(4,2,2,4),(0.118343433503666,
0.512336851960316,0.93170756803854,1.28239107793455),.UNSPECIFIED.);
#841=B_SPLINE_CURVE_WITH_KNOTS('',3,(#22906,#22907,#22908,#22909,#22910,
#22911),.UNSPECIFIED.,.F.,.F.,(4,2,4),(0.,0.138207529110136,0.257151380458292),
 .UNSPECIFIED.);
#842=B_SPLINE_CURVE_WITH_KNOTS('',3,(#22912,#22913,#22914,#22915,#22916,
#22917),.UNSPECIFIED.,.F.,.F.,(4,2,4),(0.0638119305867455,0.434740434623819,
0.895232561311264),.UNSPECIFIED.);
#843=B_SPLINE_CURVE_WITH_KNOTS('',3,(#22918,#22919,#22920,#22921,#22922,
#22923,#22924,#22925),.UNSPECIFIED.,.F.,.F.,(4,2,2,4),(0.0747583116411991,
0.415738779002339,0.772551101530305,1.04863108973718),.UNSPECIFIED.);
#844=B_SPLINE_CURVE_WITH_KNOTS('',3,(#22951,#22952,#22953,#22954,#22955,
#22956,#22957,#22958),.UNSPECIFIED.,.F.,.F.,(4,2,2,4),(0.0535030672288839,
0.137418922874274,0.199655718698583,0.252976612955408),.UNSPECIFIED.);
#845=B_SPLINE_CURVE_WITH_KNOTS('',3,(#22959,#22960,#22961,#22962,#22963,
#22964),.UNSPECIFIED.,.F.,.F.,(4,2,4),(0.0638119305867455,0.434740434623819,
0.895232561311264),.UNSPECIFIED.);
#846=B_SPLINE_CURVE_WITH_KNOTS('',3,(#22981,#22982,#22983,#22984,#22985,
#22986,#22987),.UNSPECIFIED.,.F.,.F.,(4,3,4),(0.,0.0649752557063269,0.130357085622762),
 .UNSPECIFIED.);
#847=B_SPLINE_CURVE_WITH_KNOTS('',3,(#22990,#22991,#22992,#22993,#22994,
#22995,#22996,#22997),.UNSPECIFIED.,.F.,.F.,(4,2,2,4),(0.154059232628121,
0.53443452576449,0.968745967316035,1.33329265532902),.UNSPECIFIED.);
#848=B_SPLINE_CURVE_WITH_KNOTS('',3,(#23025,#23026,#23027,#23028,#23029,
#23030),.UNSPECIFIED.,.F.,.F.,(4,2,4),(0.,0.138207529111244,0.257151380457893),
 .UNSPECIFIED.);
#849=B_SPLINE_CURVE_WITH_KNOTS('',3,(#23031,#23032,#23033,#23034,#23035,
#23036),.UNSPECIFIED.,.F.,.F.,(4,2,4),(0.0638119305867455,0.434740434623819,
0.895232561311264),.UNSPECIFIED.);
#850=B_SPLINE_CURVE_WITH_KNOTS('',3,(#23037,#23038,#23039,#23040,#23041,
#23042,#23043,#23044),.UNSPECIFIED.,.F.,.F.,(4,2,2,4),(0.074758311641198,
0.415738779002409,0.772551101530352,1.04863108973713),.UNSPECIFIED.);
#851=B_SPLINE_CURVE_WITH_KNOTS('',3,(#23070,#23071,#23072,#23073,#23074,
#23075,#23076,#23077),.UNSPECIFIED.,.F.,.F.,(4,2,2,4),(0.0535030672292633,
0.137418922876037,0.199655718701109,0.252976612961143),.UNSPECIFIED.);
#852=B_SPLINE_CURVE_WITH_KNOTS('',3,(#23078,#23079,#23080,#23081,#23082,
#23083),.UNSPECIFIED.,.F.,.F.,(4,2,4),(0.0638119305867455,0.434740434623819,
0.895232561311264),.UNSPECIFIED.);
#853=B_SPLINE_CURVE_WITH_KNOTS('',3,(#23100,#23101,#23102,#23103,#23104,
#23105,#23106),.UNSPECIFIED.,.F.,.F.,(4,3,4),(0.,0.064975255706295,0.130357085622655),
 .UNSPECIFIED.);
#854=B_SPLINE_CURVE_WITH_KNOTS('',3,(#23109,#23110,#23111,#23112,#23113,
#23114,#23115,#23116),.UNSPECIFIED.,.F.,.F.,(4,2,2,4),(0.154059232628213,
0.53443452576567,0.968745967318966,1.33329265533342),.UNSPECIFIED.);
#855=B_SPLINE_CURVE_WITH_KNOTS('',3,(#23144,#23145,#23146,#23147,#23148,
#23149),.UNSPECIFIED.,.F.,.F.,(4,2,4),(0.,0.138207529110641,0.257151380449519),
 .UNSPECIFIED.);
#856=B_SPLINE_CURVE_WITH_KNOTS('',3,(#23150,#23151,#23152,#23153,#23154,
#23155),.UNSPECIFIED.,.F.,.F.,(4,2,4),(0.0638119305867454,0.434740434623819,
0.895232561311263),.UNSPECIFIED.);
#857=B_SPLINE_CURVE_WITH_KNOTS('',3,(#23156,#23157,#23158,#23159,#23160,
#23161,#23162,#23163),.UNSPECIFIED.,.F.,.F.,(4,2,2,4),(0.0747583116411987,
0.415738779002504,0.772551101530452,1.04863108973715),.UNSPECIFIED.);
#858=B_SPLINE_CURVE_WITH_KNOTS('',3,(#23189,#23190,#23191,#23192,#23193,
#23194,#23195,#23196),.UNSPECIFIED.,.F.,.F.,(4,2,2,4),(0.0535030672291719,
0.137418922876308,0.199655718705506,0.252976612970481),.UNSPECIFIED.);
#859=B_SPLINE_CURVE_WITH_KNOTS('',3,(#23197,#23198,#23199,#23200,#23201,
#23202),.UNSPECIFIED.,.F.,.F.,(4,2,4),(0.0638119305867453,0.434740434623819,
0.895232561311264),.UNSPECIFIED.);
#860=B_SPLINE_CURVE_WITH_KNOTS('',3,(#23219,#23220,#23221,#23222,#23223,
#23224,#23225),.UNSPECIFIED.,.F.,.F.,(4,3,4),(0.,0.0649752557063512,0.130357085622858),
 .UNSPECIFIED.);
#861=B_SPLINE_CURVE_WITH_KNOTS('',3,(#23228,#23229,#23230,#23231,#23232,
#23233,#23234,#23235),.UNSPECIFIED.,.F.,.F.,(4,2,2,4),(0.15405923262826,
0.534434525766248,0.968745967320369,1.33329265533552),.UNSPECIFIED.);
#862=B_SPLINE_CURVE_WITH_KNOTS('',3,(#23263,#23264,#23265,#23266,#23267,
#23268),.UNSPECIFIED.,.F.,.F.,(4,2,4),(0.,0.138207529110164,0.257151380454439),
 .UNSPECIFIED.);
#863=B_SPLINE_CURVE_WITH_KNOTS('',3,(#23269,#23270,#23271,#23272,#23273,
#23274),.UNSPECIFIED.,.F.,.F.,(4,2,4),(0.0638119305867455,0.434740434623819,
0.895232561311264),.UNSPECIFIED.);
#864=B_SPLINE_CURVE_WITH_KNOTS('',3,(#23275,#23276,#23277,#23278,#23279,
#23280,#23281,#23282),.UNSPECIFIED.,.F.,.F.,(4,2,2,4),(0.0747583116411995,
0.415738779002478,0.772551101530437,1.04863108973718),.UNSPECIFIED.);
#865=B_SPLINE_CURVE_WITH_KNOTS('',3,(#23308,#23309,#23310,#23311,#23312,
#23313,#23314,#23315),.UNSPECIFIED.,.F.,.F.,(4,2,2,4),(0.0535030672281601,
0.137418922870713,0.199655718691404,0.252976612943466),.UNSPECIFIED.);
#866=B_SPLINE_CURVE_WITH_KNOTS('',3,(#23316,#23317,#23318,#23319,#23320,
#23321),.UNSPECIFIED.,.F.,.F.,(4,2,4),(0.0638119305867454,0.434740434623819,
0.895232561311264),.UNSPECIFIED.);
#867=B_SPLINE_CURVE_WITH_KNOTS('',3,(#23338,#23339,#23340,#23341,#23342,
#23343,#23344),.UNSPECIFIED.,.F.,.F.,(4,3,4),(0.,0.0649752557063186,0.130357085622797),
 .UNSPECIFIED.);
#868=B_SPLINE_CURVE_WITH_KNOTS('',3,(#23347,#23348,#23349,#23350,#23351,
#23352,#23353,#23354),.UNSPECIFIED.,.F.,.F.,(4,2,2,4),(0.154059232628401,
0.534434525767925,0.968745967324708,1.33329265534209),.UNSPECIFIED.);
#869=B_SPLINE_CURVE_WITH_KNOTS('',3,(#23382,#23383,#23384,#23385,#23386,
#23387),.UNSPECIFIED.,.F.,.F.,(4,2,4),(0.,0.138207529107339,0.257151380437116),
 .UNSPECIFIED.);
#870=B_SPLINE_CURVE_WITH_KNOTS('',3,(#23388,#23389,#23390,#23391,#23392,
#23393),.UNSPECIFIED.,.F.,.F.,(4,2,4),(0.0638119305867455,0.434740434623819,
0.895232561311264),.UNSPECIFIED.);
#871=B_SPLINE_CURVE_WITH_KNOTS('',3,(#23394,#23395,#23396,#23397,#23398,
#23399,#23400,#23401),.UNSPECIFIED.,.F.,.F.,(4,2,2,4),(0.0747583116412006,
0.41573877900234,0.752886816639902,1.0479630848247),.UNSPECIFIED.);
#872=B_SPLINE_CURVE_WITH_KNOTS('',3,(#23427,#23428,#23429,#23430),
 .UNSPECIFIED.,.F.,.F.,(4,4),(0.053503067228538,0.100640802838924),
 .UNSPECIFIED.);
#873=B_SPLINE_CURVE_WITH_KNOTS('',3,(#23432,#23433,#23434,#23435,#23436,
#23437),.UNSPECIFIED.,.F.,.F.,(4,2,4),(0.0638119305867455,0.434740434623819,
0.895232561311264),.UNSPECIFIED.);
#874=B_SPLINE_CURVE_WITH_KNOTS('',3,(#23438,#23439,#23440,#23441,#23442,
#23443,#23444,#23445),.UNSPECIFIED.,.F.,.F.,(4,2,2,4),(0.100640802838924,
0.13741892287284,0.199655718695611,0.252976612950919),.UNSPECIFIED.);
#875=B_SPLINE_CURVE_WITH_KNOTS('',3,(#23462,#23463,#23464,#23465,#23466,
#23467,#23468),.UNSPECIFIED.,.F.,.F.,(4,3,4),(0.,0.0649752557062351,0.130357085622553),
 .UNSPECIFIED.);
#876=B_SPLINE_CURVE_WITH_KNOTS('',3,(#23471,#23472,#23473,#23474,#23475,
#23476,#23477,#23478),.UNSPECIFIED.,.F.,.F.,(4,2,2,4),(0.11834343350374,
0.512336851961745,0.931707568042095,1.28239107793988),.UNSPECIFIED.);
#877=B_SPLINE_CURVE_WITH_KNOTS('',3,(#23506,#23507,#23508,#23509,#23510,
#23511),.UNSPECIFIED.,.F.,.F.,(4,2,4),(0.,0.138207529109375,0.257151380450338),
 .UNSPECIFIED.);
#878=B_SPLINE_CURVE_WITH_KNOTS('',3,(#23512,#23513,#23514,#23515,#23516,
#23517),.UNSPECIFIED.,.F.,.F.,(4,2,4),(0.0638119305867455,0.434740434623819,
0.895232561311264),.UNSPECIFIED.);
#879=B_SPLINE_CURVE_WITH_KNOTS('',3,(#23518,#23519,#23520,#23521,#23522,
#23523,#23524,#23525),.UNSPECIFIED.,.F.,.F.,(4,2,2,4),(0.0747583116412016,
0.415738779002347,0.772551101530358,1.04863108973731),.UNSPECIFIED.);
#880=B_SPLINE_CURVE_WITH_KNOTS('',3,(#23551,#23552,#23553,#23554,#23555,
#23556,#23557,#23558),.UNSPECIFIED.,.F.,.F.,(4,2,2,4),(0.0535030672288559,
0.13741892287429,0.199655718700123,0.252976612958485),.UNSPECIFIED.);
#881=B_SPLINE_CURVE_WITH_KNOTS('',3,(#23559,#23560,#23561,#23562,#23563,
#23564),.UNSPECIFIED.,.F.,.F.,(4,2,4),(0.0638119305867455,0.434740434623819,
0.895232561311264),.UNSPECIFIED.);
#882=B_SPLINE_CURVE_WITH_KNOTS('',3,(#23581,#23582,#23583,#23584,#23585,
#23586,#23587),.UNSPECIFIED.,.F.,.F.,(4,3,4),(0.,0.0649752557062924,0.130357085622708),
 .UNSPECIFIED.);
#883=B_SPLINE_CURVE_WITH_KNOTS('',3,(#23590,#23591,#23592,#23593,#23594,
#23595,#23596,#23597),.UNSPECIFIED.,.F.,.F.,(4,2,2,4),(0.154059232628241,
0.534434525766006,0.968745967319776,1.33329265533462),.UNSPECIFIED.);
#884=B_SPLINE_CURVE_WITH_KNOTS('',3,(#23625,#23626,#23627,#23628,#23629,
#23630),.UNSPECIFIED.,.F.,.F.,(4,2,4),(0.,0.138207529111243,0.257151380457902),
 .UNSPECIFIED.);
#885=B_SPLINE_CURVE_WITH_KNOTS('',3,(#23631,#23632,#23633,#23634,#23635,
#23636),.UNSPECIFIED.,.F.,.F.,(4,2,4),(0.0638119305867455,0.434740434623819,
0.895232561311264),.UNSPECIFIED.);
#886=B_SPLINE_CURVE_WITH_KNOTS('',3,(#23637,#23638,#23639,#23640,#23641,
#23642,#23643,#23644),.UNSPECIFIED.,.F.,.F.,(4,2,2,4),(0.0747583116411995,
0.415738779002564,0.772551101530526,1.04863108973719),.UNSPECIFIED.);
#887=B_SPLINE_CURVE_WITH_KNOTS('',3,(#23670,#23671,#23672,#23673,#23674,
#23675,#23676,#23677),.UNSPECIFIED.,.F.,.F.,(4,2,2,4),(0.0535030672292643,
0.13741892287604,0.199655718701115,0.252976612961142),.UNSPECIFIED.);
#888=B_SPLINE_CURVE_WITH_KNOTS('',3,(#23678,#23679,#23680,#23681,#23682,
#23683),.UNSPECIFIED.,.F.,.F.,(4,2,4),(0.0638119305867455,0.434740434623819,
0.895232561311264),.UNSPECIFIED.);
#889=B_SPLINE_CURVE_WITH_KNOTS('',3,(#23700,#23701,#23702,#23703,#23704,
#23705,#23706),.UNSPECIFIED.,.F.,.F.,(4,3,4),(0.,0.0649752557062854,0.130357085622667),
 .UNSPECIFIED.);
#890=B_SPLINE_CURVE_WITH_KNOTS('',3,(#23709,#23710,#23711,#23712,#23713,
#23714,#23715,#23716),.UNSPECIFIED.,.F.,.F.,(4,2,2,4),(0.154059232628168,
0.534434525765134,0.968745967317506,1.33329265533118),.UNSPECIFIED.);
#891=B_SPLINE_CURVE_WITH_KNOTS('',3,(#23744,#23745,#23746,#23747,#23748,
#23749),.UNSPECIFIED.,.F.,.F.,(4,2,4),(0.,0.138207529112972,0.257151380462745),
 .UNSPECIFIED.);
#892=B_SPLINE_CURVE_WITH_KNOTS('',3,(#23750,#23751,#23752,#23753,#23754,
#23755),.UNSPECIFIED.,.F.,.F.,(4,2,4),(0.0638119305867454,0.434740434623819,
0.895232561311263),.UNSPECIFIED.);
#893=B_SPLINE_CURVE_WITH_KNOTS('',3,(#23756,#23757,#23758,#23759,#23760,
#23761,#23762,#23763),.UNSPECIFIED.,.F.,.F.,(4,2,2,4),(0.0747583116411983,
0.415738779002571,0.772551101530515,1.04863108973714),.UNSPECIFIED.);
#894=B_SPLINE_CURVE_WITH_KNOTS('',3,(#23789,#23790,#23791,#23792,#23793,
#23794,#23795,#23796),.UNSPECIFIED.,.F.,.F.,(4,2,2,4),(0.0535030672291713,
0.137418922876305,0.199655718705507,0.252976612970469),.UNSPECIFIED.);
#895=B_SPLINE_CURVE_WITH_KNOTS('',3,(#23797,#23798,#23799,#23800,#23801,
#23802),.UNSPECIFIED.,.F.,.F.,(4,2,4),(0.0638119305867453,0.434740434623819,
0.895232561311264),.UNSPECIFIED.);
#896=B_SPLINE_CURVE_WITH_KNOTS('',3,(#23819,#23820,#23821,#23822,#23823,
#23824,#23825),.UNSPECIFIED.,.F.,.F.,(4,3,4),(0.,0.0649752557062912,0.130357085622682),
 .UNSPECIFIED.);
#897=B_SPLINE_CURVE_WITH_KNOTS('',3,(#23828,#23829,#23830,#23831,#23832,
#23833,#23834,#23835),.UNSPECIFIED.,.F.,.F.,(4,2,2,4),(0.154059232628393,
0.534434525767844,0.968745967324445,1.33329265534166),.UNSPECIFIED.);
#898=B_SPLINE_CURVE_WITH_KNOTS('',3,(#23863,#23864,#23865,#23866,#23867,
#23868),.UNSPECIFIED.,.F.,.F.,(4,2,4),(0.,0.138207529110578,0.257151380453696),
 .UNSPECIFIED.);
#899=B_SPLINE_CURVE_WITH_KNOTS('',3,(#23869,#23870,#23871,#23872,#23873,
#23874),.UNSPECIFIED.,.F.,.F.,(4,2,4),(0.0638119305867454,0.434740434623819,
0.895232561311264),.UNSPECIFIED.);
#900=B_SPLINE_CURVE_WITH_KNOTS('',3,(#23875,#23876,#23877,#23878,#23879,
#23880,#23881,#23882),.UNSPECIFIED.,.F.,.F.,(4,2,2,4),(0.0747583116412008,
0.415738779002461,0.77255110153044,1.04863108973723),.UNSPECIFIED.);
#901=B_SPLINE_CURVE_WITH_KNOTS('',3,(#23908,#23909,#23910,#23911,#23912,
#23913,#23914,#23915),.UNSPECIFIED.,.F.,.F.,(4,2,2,4),(0.0535030672281967,
0.137418922870822,0.199655718691029,0.252976612941727),.UNSPECIFIED.);
#902=B_SPLINE_CURVE_WITH_KNOTS('',3,(#23916,#23917,#23918,#23919,#23920,
#23921),.UNSPECIFIED.,.F.,.F.,(4,2,4),(0.0638119305867454,0.434740434623819,
0.895232561311264),.UNSPECIFIED.);
#903=B_SPLINE_CURVE_WITH_KNOTS('',3,(#23938,#23939,#23940,#23941,#23942,
#23943,#23944),.UNSPECIFIED.,.F.,.F.,(4,3,4),(0.,0.0649752557062974,0.130357085622712),
 .UNSPECIFIED.);
#904=B_SPLINE_CURVE_WITH_KNOTS('',3,(#23947,#23948,#23949,#23950,#23951,
#23952,#23953,#23954),.UNSPECIFIED.,.F.,.F.,(4,2,2,4),(0.154059232628199,
0.534434525765498,0.968745967318458,1.33329265533263),.UNSPECIFIED.);
#905=B_SPLINE_CURVE_WITH_KNOTS('',3,(#23982,#23983,#23984,#23985,#23986,
#23987),.UNSPECIFIED.,.F.,.F.,(4,2,4),(0.,0.138207529113734,0.257151380471648),
 .UNSPECIFIED.);
#906=B_SPLINE_CURVE_WITH_KNOTS('',3,(#23988,#23989,#23990,#23991,#23992,
#23993),.UNSPECIFIED.,.F.,.F.,(4,2,4),(0.0638119305867455,0.434740434623819,
0.895232561311264),.UNSPECIFIED.);
#907=B_SPLINE_CURVE_WITH_KNOTS('',3,(#23994,#23995,#23996,#23997,#23998,
#23999,#24000,#24001),.UNSPECIFIED.,.F.,.F.,(4,2,2,4),(0.074758311641198,
0.41573877900249,0.752886816639918,1.0479630848246),.UNSPECIFIED.);
#908=B_SPLINE_CURVE_WITH_KNOTS('',3,(#24027,#24028,#24029,#24030,#24031,
#24032,#24033,#24034),.UNSPECIFIED.,.F.,.F.,(4,2,2,4),(0.0535030672285459,
0.137418922872875,0.199655718695463,0.252976612950634),.UNSPECIFIED.);
#909=B_SPLINE_CURVE_WITH_KNOTS('',3,(#24035,#24036,#24037,#24038,#24039,
#24040),.UNSPECIFIED.,.F.,.F.,(4,2,4),(0.0638119305867455,0.434740434623819,
0.895232561311264),.UNSPECIFIED.);
#910=B_SPLINE_CURVE_WITH_KNOTS('',3,(#24057,#24058,#24059,#24060,#24061,
#24062,#24063),.UNSPECIFIED.,.F.,.F.,(4,3,4),(0.,0.0649752557063032,0.130357085622734),
 .UNSPECIFIED.);
#911=B_SPLINE_CURVE_WITH_KNOTS('',3,(#24066,#24067,#24068,#24069,#24070,
#24071,#24072,#24073),.UNSPECIFIED.,.F.,.F.,(4,2,2,4),(0.118343433503678,
0.512336851960549,0.931707568039129,1.28239107793543),.UNSPECIFIED.);
#912=B_SPLINE_CURVE_WITH_KNOTS('',3,(#24101,#24102,#24103,#24104,#24105,
#24106),.UNSPECIFIED.,.F.,.F.,(4,2,4),(0.,0.138207529112825,0.257151380461063),
 .UNSPECIFIED.);
#913=B_SPLINE_CURVE_WITH_KNOTS('',3,(#24107,#24108,#24109,#24110,#24111,
#24112),.UNSPECIFIED.,.F.,.F.,(4,2,4),(0.0638119305867454,0.434740434623819,
0.895232561311264),.UNSPECIFIED.);
#914=B_SPLINE_CURVE_WITH_KNOTS('',3,(#24113,#24114,#24115,#24116,#24117,
#24118,#24119,#24120),.UNSPECIFIED.,.F.,.F.,(4,2,2,4),(0.0747583116412005,
0.415738779002413,0.772551101530409,1.04863108973728),.UNSPECIFIED.);
#915=B_SPLINE_CURVE_WITH_KNOTS('',3,(#24146,#24147,#24148,#24149,#24150,
#24151,#24152,#24153),.UNSPECIFIED.,.F.,.F.,(4,2,2,4),(0.0535030672285232,
0.137418922872583,0.199655718694823,0.252976612949017),.UNSPECIFIED.);
#916=B_SPLINE_CURVE_WITH_KNOTS('',3,(#24154,#24155,#24156,#24157,#24158,
#24159),.UNSPECIFIED.,.F.,.F.,(4,2,4),(0.0638119305867454,0.434740434623819,
0.895232561311264),.UNSPECIFIED.);
#917=B_SPLINE_CURVE_WITH_KNOTS('',3,(#24176,#24177,#24178,#24179,#24180,
#24181,#24182),.UNSPECIFIED.,.F.,.F.,(4,3,4),(0.,0.0649752557062746,0.130357085622654),
 .UNSPECIFIED.);
#918=B_SPLINE_CURVE_WITH_KNOTS('',3,(#24185,#24186,#24187,#24188,#24189,
#24190,#24191,#24192),.UNSPECIFIED.,.F.,.F.,(4,2,2,4),(0.154059232628271,
0.534434525766387,0.968745967320721,1.33329265533604),.UNSPECIFIED.);
#919=B_SPLINE_CURVE_WITH_KNOTS('',3,(#24220,#24221,#24222,#24223,#24224,
#24225),.UNSPECIFIED.,.F.,.F.,(4,2,4),(0.,0.138207529114044,0.257151380464847),
 .UNSPECIFIED.);
#920=B_SPLINE_CURVE_WITH_KNOTS('',3,(#24226,#24227,#24228,#24229,#24230,
#24231),.UNSPECIFIED.,.F.,.F.,(4,2,4),(0.0638119305867455,0.434740434623819,
0.895232561311264),.UNSPECIFIED.);
#921=B_SPLINE_CURVE_WITH_KNOTS('',3,(#24232,#24233,#24234,#24235,#24236,
#24237,#24238,#24239),.UNSPECIFIED.,.F.,.F.,(4,2,2,4),(0.0747583116412018,
0.415738779002431,0.772551101530457,1.04863108973735),.UNSPECIFIED.);
#922=B_SPLINE_CURVE_WITH_KNOTS('',3,(#24265,#24266,#24267,#24268,#24269,
#24270,#24271,#24272),.UNSPECIFIED.,.F.,.F.,(4,2,2,4),(0.053503067228947,
0.137418922874791,0.199655718705812,0.252976612970407),.UNSPECIFIED.);
#923=B_SPLINE_CURVE_WITH_KNOTS('',3,(#24273,#24274,#24275,#24276,#24277,
#24278),.UNSPECIFIED.,.F.,.F.,(4,2,4),(0.0638119305867455,0.434740434623819,
0.895232561311264),.UNSPECIFIED.);
#924=B_SPLINE_CURVE_WITH_KNOTS('',3,(#24295,#24296,#24297,#24298,#24299,
#24300,#24301),.UNSPECIFIED.,.F.,.F.,(4,3,4),(0.,0.0649752557062623,0.130357085622632),
 .UNSPECIFIED.);
#925=B_SPLINE_CURVE_WITH_KNOTS('',3,(#24304,#24305,#24306,#24307,#24308,
#24309,#24310,#24311),.UNSPECIFIED.,.F.,.F.,(4,2,2,4),(0.154059232628193,
0.534434525765401,0.968745967318279,1.33329265533237),.UNSPECIFIED.);
#926=B_SPLINE_CURVE_WITH_KNOTS('',3,(#24339,#24340,#24341,#24342,#24343,
#24344),.UNSPECIFIED.,.F.,.F.,(4,2,4),(0.,0.13820752911105,0.257151380454454),
 .UNSPECIFIED.);
#927=B_SPLINE_CURVE_WITH_KNOTS('',3,(#24345,#24346,#24347,#24348,#24349,
#24350),.UNSPECIFIED.,.F.,.F.,(4,2,4),(0.0638119305867455,0.434740434623819,
0.895232561311264),.UNSPECIFIED.);
#928=B_SPLINE_CURVE_WITH_KNOTS('',3,(#24351,#24352,#24353,#24354,#24355,
#24356,#24357,#24358),.UNSPECIFIED.,.F.,.F.,(4,2,2,4),(0.074758311641201,
0.415738779002626,0.772551101530626,1.0486310897373),.UNSPECIFIED.);
#929=B_SPLINE_CURVE_WITH_KNOTS('',3,(#24384,#24385,#24386,#24387,#24388,
#24389,#24390,#24391),.UNSPECIFIED.,.F.,.F.,(4,2,2,4),(0.0535030672290782,
0.137418922874952,0.199655718700024,0.252976612958131),.UNSPECIFIED.);
#930=B_SPLINE_CURVE_WITH_KNOTS('',3,(#24392,#24393,#24394,#24395,#24396,
#24397),.UNSPECIFIED.,.F.,.F.,(4,2,4),(0.0638119305867455,0.434740434623819,
0.895232561311264),.UNSPECIFIED.);
#931=B_SPLINE_CURVE_WITH_KNOTS('',3,(#24414,#24415,#24416,#24417,#24418,
#24419,#24420),.UNSPECIFIED.,.F.,.F.,(4,3,4),(0.,0.0649752557062915,0.130357085622713),
 .UNSPECIFIED.);
#932=B_SPLINE_CURVE_WITH_KNOTS('',3,(#24423,#24424,#24425,#24426,#24427,
#24428,#24429,#24430),.UNSPECIFIED.,.F.,.F.,(4,2,2,4),(0.154059232628257,
0.534434525766122,0.968745967320132,1.33329265533518),.UNSPECIFIED.);
#933=B_SPLINE_CURVE_WITH_KNOTS('',3,(#24457,#24458,#24459,#24460,#24461,
#24462),.UNSPECIFIED.,.F.,.F.,(4,2,4),(0.0638119305867453,0.434740434623819,
0.895232561311263),.UNSPECIFIED.);
#934=B_SPLINE_CURVE_WITH_KNOTS('',3,(#24463,#24464,#24465,#24466,#24467,
#24468,#24469,#24470),.UNSPECIFIED.,.F.,.F.,(4,2,2,4),(0.0535030672280216,
0.137418922870031,0.199655718689467,0.2529766129386),.UNSPECIFIED.);
#935=B_SPLINE_CURVE_WITH_KNOTS('',3,(#24488,#24489,#24490,#24491,#24492,
#24493),.UNSPECIFIED.,.F.,.F.,(4,2,4),(0.0638119305867453,0.434740434623819,
0.895232561311264),.UNSPECIFIED.);
#936=B_SPLINE_CURVE_WITH_KNOTS('',3,(#24494,#24495,#24496,#24497,#24498,
#24499,#24500),.UNSPECIFIED.,.F.,.F.,(4,3,4),(0.,0.0649752557062552,0.130357085622604),
 .UNSPECIFIED.);
#937=B_SPLINE_CURVE_WITH_KNOTS('',3,(#24526,#24527,#24528,#24529,#24530,
#24531,#24532,#24533),.UNSPECIFIED.,.F.,.F.,(4,2,2,4),(0.074758311641199,
0.415738779002503,0.77255110153046,1.04863108973717),.UNSPECIFIED.);
#938=B_SPLINE_CURVE_WITH_KNOTS('',3,(#24534,#24535,#24536,#24537,#24538,
#24539),.UNSPECIFIED.,.F.,.F.,(4,2,4),(0.,0.138207529110333,0.257151380458365),
 .UNSPECIFIED.);
#939=B_SPLINE_CURVE_WITH_KNOTS('',3,(#24565,#24566,#24567,#24568,#24569,
#24570),.UNSPECIFIED.,.F.,.F.,(4,2,4),(0.0638119305867455,0.434740434623819,
0.895232561311264),.UNSPECIFIED.);
#940=B_SPLINE_CURVE_WITH_KNOTS('',3,(#24572,#24573,#24574,#24575,#24576,
#24577,#24578,#24579),.UNSPECIFIED.,.F.,.F.,(4,2,2,4),(0.0535030672285654,
0.137418922872966,0.199655718695898,0.252976612951402),.UNSPECIFIED.);
#941=B_SPLINE_CURVE_WITH_KNOTS('',3,(#24580,#24581,#24582,#24583,#24584,
#24585,#24586,#24587),.UNSPECIFIED.,.F.,.F.,(4,2,2,4),(0.154059232628261,
0.534434525766262,0.96874596732043,1.33329265533561),.UNSPECIFIED.);
#942=B_SPLINE_CURVE_WITH_KNOTS('',3,(#24605,#24606,#24607,#24608,#24609,
#24610),.UNSPECIFIED.,.F.,.F.,(4,2,4),(0.0638119305867455,0.434740434623819,
0.895232561311264),.UNSPECIFIED.);
#943=B_SPLINE_CURVE_WITH_KNOTS('',3,(#24611,#24612,#24613,#24614,#24615,
#24616,#24617),.UNSPECIFIED.,.F.,.F.,(4,3,4),(0.,0.0649752557063237,0.130357085622785),
 .UNSPECIFIED.);
#944=B_SPLINE_CURVE_WITH_KNOTS('',3,(#24642,#24643,#24644,#24645,#24646,
#24647),.UNSPECIFIED.,.F.,.F.,(4,2,4),(0.,0.13820752910729,0.257151380436842),
 .UNSPECIFIED.);
#945=B_SPLINE_CURVE_WITH_KNOTS('',3,(#24703,#24704,#24705,#24706,#24707,
#24708),.UNSPECIFIED.,.F.,.F.,(4,2,4),(0.254797907722713,0.274731256245471,
0.294664604768228),.UNSPECIFIED.);
#946=B_SPLINE_CURVE_WITH_KNOTS('',3,(#24712,#24713,#24714,#24715,#24716,
#24717),.UNSPECIFIED.,.F.,.F.,(4,2,4),(0.254797907722713,0.274731256245471,
0.294664604768229),.UNSPECIFIED.);
#947=B_SPLINE_CURVE_WITH_KNOTS('',3,(#24721,#24722,#24723,#24724,#24725,
#24726),.UNSPECIFIED.,.F.,.F.,(4,2,4),(0.254797907722713,0.274731256245471,
0.294664604768229),.UNSPECIFIED.);
#948=B_SPLINE_CURVE_WITH_KNOTS('',3,(#24730,#24731,#24732,#24733,#24734,
#24735),.UNSPECIFIED.,.F.,.F.,(4,2,4),(0.254797907722713,0.274731256245471,
0.294664604768228),.UNSPECIFIED.);
#949=B_SPLINE_CURVE_WITH_KNOTS('',3,(#24739,#24740,#24741,#24742,#24743,
#24744),.UNSPECIFIED.,.F.,.F.,(4,2,4),(0.254797907722728,0.274731256245471,
0.294664604768213),.UNSPECIFIED.);
#950=B_SPLINE_CURVE_WITH_KNOTS('',3,(#24751,#24752,#24753,#24754,#24755,
#24756),.UNSPECIFIED.,.F.,.F.,(4,2,4),(0.254797907722713,0.274731256245471,
0.294664604768229),.UNSPECIFIED.);
#951=B_SPLINE_CURVE_WITH_KNOTS('',3,(#24760,#24761,#24762,#24763,#24764,
#24765),.UNSPECIFIED.,.F.,.F.,(4,2,4),(0.254797907722728,0.274731256245471,
0.294664604768213),.UNSPECIFIED.);
#952=B_SPLINE_CURVE_WITH_KNOTS('',3,(#24770,#24771,#24772,#24773),
 .UNSPECIFIED.,.F.,.F.,(4,4),(0.750997797800867,0.767662411819255),
 .UNSPECIFIED.);
#953=B_SPLINE_CURVE_WITH_KNOTS('',3,(#24775,#24776,#24777,#24778,#24779,
#24780,#24781,#24782,#24783,#24784,#24785,#24786,#24787,#24788,#24789,#24790,
#24791,#24792,#24793,#24794,#24795,#24796),.UNSPECIFIED.,.F.,.F.,(4,2,2,
2,2,2,2,2,2,2,4),(0.516725915130786,0.527390969880923,0.571339243451659,
0.615287517022395,0.659234130021226,0.703180743020057,0.747127356018888,
0.791073969017719,0.835022242588455,0.878970516159191,0.889635570909327),
 .UNSPECIFIED.);
#954=B_SPLINE_CURVE_WITH_KNOTS('',3,(#24798,#24799,#24800,#24801),
 .UNSPECIFIED.,.F.,.F.,(4,4),(0.255887470606418,0.272552084624806),
 .UNSPECIFIED.);
#955=B_SPLINE_CURVE_WITH_KNOTS('',3,(#24805,#24806,#24807,#24808),
 .UNSPECIFIED.,.F.,.F.,(4,4),(0.239222856588031,0.255887470606418),
 .UNSPECIFIED.);
#956=B_SPLINE_CURVE_WITH_KNOTS('',3,(#24810,#24811,#24812,#24813,#24814,
#24815,#24816,#24817,#24818,#24819,#24820,#24821,#24822,#24823,#24824,#24825,
#24826,#24827,#24828,#24829,#24830,#24831),.UNSPECIFIED.,.F.,.F.,(4,2,2,
2,2,2,2,2,2,2,4),(0.516725915130786,0.527390969880923,0.571339243451659,
0.615287517022395,0.659234130021226,0.703180743020057,0.747127356018888,
0.791073969017718,0.835022242588455,0.878970516159191,0.889635570909327),
 .UNSPECIFIED.);
#957=B_SPLINE_CURVE_WITH_KNOTS('',3,(#24832,#24833,#24834,#24835),
 .UNSPECIFIED.,.F.,.F.,(4,4),(0.767662411819255,0.784327025837643),
 .UNSPECIFIED.);
#958=B_SPLINE_CURVE_WITH_KNOTS('',3,(#24839,#24840,#24841,#24842,#24843,
#24844,#24845,#24846,#24847,#24848,#24849,#24850,#24851,#24852,#24853,#24854,
#24855,#24856,#24857,#24858,#24859,#24860,#24861),.UNSPECIFIED.,.F.,.F.,
(4,2,2,2,2,3,2,2,2,2,4),(-0.186453873187253,-0.17578960100413,-0.131841711164795,
-0.087893821325461,-0.0439469106627304,0.,0.0439469106627304,0.0878938213254609,
0.131841711164795,0.17578960100413,0.186453873187381),.UNSPECIFIED.);
#959=B_SPLINE_CURVE_WITH_KNOTS('',3,(#24863,#24864,#24865,#24866,#24867,
#24868),.UNSPECIFIED.,.F.,.F.,(4,2,4),(0.804260420213654,0.824193768736411,
0.844127117259169),.UNSPECIFIED.);
#960=B_SPLINE_CURVE_WITH_KNOTS('',3,(#24869,#24870,#24871,#24872,#24873,
#24874,#24875,#24876,#24877,#24878,#24879,#24880,#24881,#24882,#24883,#24884,
#24885,#24886,#24887,#24888,#24889,#24890,#24891),.UNSPECIFIED.,.F.,.F.,
(4,2,2,2,2,3,2,2,2,2,4),(-0.186453873187253,-0.17578960100413,-0.131841711164795,
-0.087893821325461,-0.0439469106627306,0.,0.0439469106627304,0.0878938213254609,
0.131841711164795,0.17578960100413,0.186453873187381),.UNSPECIFIED.);
#961=B_SPLINE_CURVE_WITH_KNOTS('',3,(#24898,#24899,#24900,#24901,#24902,
#24903),.UNSPECIFIED.,.F.,.F.,(4,2,4),(0.804260420213644,0.824193768736412,
0.84412711725918),.UNSPECIFIED.);
#962=B_SPLINE_CURVE_WITH_KNOTS('',3,(#24907,#24908,#24909,#24910,#24911,
#24912),.UNSPECIFIED.,.F.,.F.,(4,2,4),(0.804260420213654,0.824193768736412,
0.84412711725917),.UNSPECIFIED.);
#963=B_SPLINE_CURVE_WITH_KNOTS('',3,(#24916,#24917,#24918,#24919,#24920,
#24921),.UNSPECIFIED.,.F.,.F.,(4,2,4),(0.804260420213654,0.824193768736411,
0.844127117259169),.UNSPECIFIED.);
#964=B_SPLINE_CURVE_WITH_KNOTS('',3,(#24925,#24926,#24927,#24928,#24929,
#24930),.UNSPECIFIED.,.F.,.F.,(4,2,4),(0.804260420213654,0.824193768736411,
0.844127117259169),.UNSPECIFIED.);
#965=B_SPLINE_CURVE_WITH_KNOTS('',3,(#24935,#24936,#24937,#24938,#24939,
#24940),.UNSPECIFIED.,.F.,.F.,(4,2,4),(0.804260420213643,0.824193768736411,
0.844127117259179),.UNSPECIFIED.);
#966=B_SPLINE_CURVE_WITH_KNOTS('',3,(#24944,#24945,#24946,#24947,#24948,
#24949),.UNSPECIFIED.,.F.,.F.,(4,2,4),(0.804260420213654,0.824193768736412,
0.844127117259169),.UNSPECIFIED.);
#967=B_SPLINE_CURVE_WITH_KNOTS('',3,(#24952,#24953,#24954,#24955,#24956,
#24957,#24958,#24959,#24960,#24961,#24962,#24963,#24964,#24965,#24966,#24967,
#24968,#24969,#24970,#24971,#24972,#24973,#24974),.UNSPECIFIED.,.F.,.F.,
(4,2,2,2,2,3,2,2,2,2,4),(-0.186453873187254,-0.17578960100413,-0.131841711164795,
-0.087893821325461,-0.0439469106627304,0.,0.0439469106627307,0.0878938213254614,
0.131841711164796,0.17578960100413,0.186453873187382),.UNSPECIFIED.);
#968=B_SPLINE_CURVE_WITH_KNOTS('',3,(#24979,#24980,#24981,#24982),
 .UNSPECIFIED.,.F.,.F.,(4,4),(0.23922285658804,0.255887470606418),
 .UNSPECIFIED.);
#969=B_SPLINE_CURVE_WITH_KNOTS('',3,(#24984,#24985,#24986,#24987),
 .UNSPECIFIED.,.F.,.F.,(4,4),(0.255887470606418,0.272552084624797),
 .UNSPECIFIED.);
#970=B_SPLINE_CURVE_WITH_KNOTS('',3,(#24991,#24992,#24993,#24994),
 .UNSPECIFIED.,.F.,.F.,(4,4),(0.239222856588031,0.255887470606418),
 .UNSPECIFIED.);
#971=B_SPLINE_CURVE_WITH_KNOTS('',3,(#24996,#24997,#24998,#24999),
 .UNSPECIFIED.,.F.,.F.,(4,4),(0.255887470606418,0.272552084624806),
 .UNSPECIFIED.);
#972=B_SPLINE_CURVE_WITH_KNOTS('',3,(#25008,#25009,#25010,#25011),
 .UNSPECIFIED.,.F.,.F.,(4,4),(0.239222856588039,0.255887470606418),
 .UNSPECIFIED.);
#973=B_SPLINE_CURVE_WITH_KNOTS('',3,(#25013,#25014,#25015,#25016),
 .UNSPECIFIED.,.F.,.F.,(4,4),(0.255887470606418,0.272552084624797),
 .UNSPECIFIED.);
#974=B_SPLINE_CURVE_WITH_KNOTS('',3,(#25020,#25021,#25022,#25023),
 .UNSPECIFIED.,.F.,.F.,(4,4),(0.239222856588031,0.255887470606418),
 .UNSPECIFIED.);
#975=B_SPLINE_CURVE_WITH_KNOTS('',3,(#25025,#25026,#25027,#25028),
 .UNSPECIFIED.,.F.,.F.,(4,4),(0.255887470606418,0.272552084624806),
 .UNSPECIFIED.);
#976=B_SPLINE_CURVE_WITH_KNOTS('',3,(#25032,#25033,#25034,#25035),
 .UNSPECIFIED.,.F.,.F.,(4,4),(0.239222856588031,0.255887470606418),
 .UNSPECIFIED.);
#977=B_SPLINE_CURVE_WITH_KNOTS('',3,(#25037,#25038,#25039,#25040),
 .UNSPECIFIED.,.F.,.F.,(4,4),(0.255887470606418,0.272552084624806),
 .UNSPECIFIED.);
#978=B_SPLINE_CURVE_WITH_KNOTS('',3,(#25044,#25045,#25046,#25047),
 .UNSPECIFIED.,.F.,.F.,(4,4),(0.239222856588031,0.255887470606418),
 .UNSPECIFIED.);
#979=B_SPLINE_CURVE_WITH_KNOTS('',3,(#25049,#25050,#25051,#25052),
 .UNSPECIFIED.,.F.,.F.,(4,4),(0.255887470606418,0.272552084624806),
 .UNSPECIFIED.);
#980=B_SPLINE_CURVE_WITH_KNOTS('',3,(#25057,#25058,#25059,#25060,#25061,
#25062,#25063,#25064,#25065,#25066,#25067,#25068,#25069,#25070,#25071,#25072,
#25073,#25074,#25075,#25076,#25077,#25078),.UNSPECIFIED.,.F.,.F.,(4,2,2,
2,2,2,2,2,2,2,4),(0.516725915130786,0.527390969880923,0.571339243451659,
0.615287517022395,0.659234130021226,0.703180743020057,0.747127356018888,
0.791073969017719,0.835022242588455,0.878970516159191,0.889635570909327),
 .UNSPECIFIED.);
#981=B_SPLINE_CURVE_WITH_KNOTS('',3,(#25082,#25083,#25084,#25085),
 .UNSPECIFIED.,.F.,.F.,(4,4),(0.750997797800864,0.767662411819255),
 .UNSPECIFIED.);
#982=B_SPLINE_CURVE_WITH_KNOTS('',3,(#25086,#25087,#25088,#25089,#25090,
#25091,#25092,#25093,#25094,#25095,#25096,#25097,#25098,#25099,#25100,#25101,
#25102,#25103,#25104,#25105,#25106,#25107),.UNSPECIFIED.,.F.,.F.,(4,2,2,
2,2,2,2,2,2,2,4),(0.516725915130786,0.527390969880923,0.571339243451659,
0.615287517022395,0.659234130021226,0.703180743020056,0.747127356018887,
0.791073969017719,0.835022242588454,0.87897051615919,0.889635570909327),
 .UNSPECIFIED.);
#983=B_SPLINE_CURVE_WITH_KNOTS('',3,(#25110,#25111,#25112,#25113),
 .UNSPECIFIED.,.F.,.F.,(4,4),(0.767662411819255,0.784327025837645),
 .UNSPECIFIED.);
#984=B_SPLINE_CURVE_WITH_KNOTS('',3,(#25116,#25117,#25118,#25119,#25120,
#25121,#25122,#25123,#25124,#25125,#25126,#25127,#25128,#25129,#25130,#25131,
#25132,#25133,#25134,#25135,#25136,#25137,#25138),.UNSPECIFIED.,.F.,.F.,
(4,2,2,2,2,3,2,2,2,2,4),(-0.186453873187254,-0.17578960100413,-0.131841711164796,
-0.0878938213254614,-0.0439469106627306,0.,0.0439469106627305,0.0878938213254609,
0.131841711164795,0.175789601004129,0.186453873187382),.UNSPECIFIED.);
#985=B_SPLINE_CURVE_WITH_KNOTS('',3,(#25140,#25141,#25142,#25143,#25144,
#25145,#25146,#25147,#25148,#25149,#25150,#25151,#25152,#25153,#25154,#25155,
#25156,#25157,#25158,#25159,#25160,#25161,#25162),.UNSPECIFIED.,.F.,.F.,
(4,2,2,2,2,3,2,2,2,2,4),(-0.186453873187253,-0.17578960100413,-0.131841711164795,
-0.087893821325461,-0.0439469106627306,0.,0.0439469106627305,0.0878938213254609,
0.131841711164795,0.17578960100413,0.186453873187381),.UNSPECIFIED.);
#986=B_SPLINE_CURVE_WITH_KNOTS('',3,(#25166,#25167,#25168,#25169,#25170,
#25171,#25172,#25173,#25174,#25175,#25176,#25177,#25178,#25179,#25180,#25181,
#25182,#25183,#25184,#25185,#25186,#25187),.UNSPECIFIED.,.F.,.F.,(4,2,2,
2,2,2,2,2,2,2,4),(0.516725915130786,0.527390969880923,0.571339243451659,
0.615287517022395,0.659234130021226,0.703180743020057,0.747127356018888,
0.791073969017718,0.835022242588455,0.878970516159191,0.889635570909327),
 .UNSPECIFIED.);
#987=B_SPLINE_CURVE_WITH_KNOTS('',3,(#25191,#25192,#25193,#25194),
 .UNSPECIFIED.,.F.,.F.,(4,4),(0.750997797800867,0.767662411819255),
 .UNSPECIFIED.);
#988=B_SPLINE_CURVE_WITH_KNOTS('',3,(#25195,#25196,#25197,#25198,#25199,
#25200,#25201,#25202,#25203,#25204,#25205,#25206,#25207,#25208,#25209,#25210,
#25211,#25212,#25213,#25214,#25215,#25216),.UNSPECIFIED.,.F.,.F.,(4,2,2,
2,2,2,2,2,2,2,4),(0.516725915130786,0.527390969880923,0.571339243451659,
0.615287517022395,0.659234130021226,0.703180743020057,0.747127356018888,
0.791073969017718,0.835022242588454,0.87897051615919,0.889635570909327),
 .UNSPECIFIED.);
#989=B_SPLINE_CURVE_WITH_KNOTS('',3,(#25219,#25220,#25221,#25222),
 .UNSPECIFIED.,.F.,.F.,(4,4),(0.767662411819255,0.784327025837642),
 .UNSPECIFIED.);
#990=B_SPLINE_CURVE_WITH_KNOTS('',3,(#25225,#25226,#25227,#25228,#25229,
#25230,#25231,#25232,#25233,#25234,#25235,#25236,#25237,#25238,#25239,#25240,
#25241,#25242,#25243,#25244,#25245,#25246,#25247),.UNSPECIFIED.,.F.,.F.,
(4,2,2,2,2,3,2,2,2,2,4),(-0.186453873187253,-0.17578960100413,-0.131841711164795,
-0.0878938213254608,-0.0439469106627304,0.,0.0439469106627304,0.0878938213254609,
0.131841711164795,0.17578960100413,0.186453873187381),.UNSPECIFIED.);
#991=B_SPLINE_CURVE_WITH_KNOTS('',3,(#25249,#25250,#25251,#25252,#25253,
#25254,#25255,#25256,#25257,#25258,#25259,#25260,#25261,#25262,#25263,#25264,
#25265,#25266,#25267,#25268,#25269,#25270,#25271),.UNSPECIFIED.,.F.,.F.,
(4,2,2,2,2,3,2,2,2,2,4),(-0.186453873187254,-0.17578960100413,-0.131841711164796,
-0.0878938213254614,-0.0439469106627308,0.,0.0439469106627309,0.0878938213254618,
0.131841711164796,0.17578960100413,0.186453873187382),.UNSPECIFIED.);
#992=B_SPLINE_CURVE_WITH_KNOTS('',3,(#25277,#25278,#25279,#25280,#25281,
#25282,#25283,#25284,#25285,#25286,#25287,#25288,#25289,#25290,#25291,#25292,
#25293,#25294,#25295,#25296,#25297,#25298),.UNSPECIFIED.,.F.,.F.,(4,2,2,
2,2,2,2,2,2,2,4),(0.516725915130787,0.527390969880924,0.571339243451659,
0.615287517022395,0.659234130021226,0.703180743020058,0.747127356018888,
0.791073969017719,0.835022242588455,0.878970516159191,0.889635570909328),
 .UNSPECIFIED.);
#993=B_SPLINE_CURVE_WITH_KNOTS('',3,(#25302,#25303,#25304,#25305),
 .UNSPECIFIED.,.F.,.F.,(4,4),(0.750997797800863,0.767662411819254),
 .UNSPECIFIED.);
#994=B_SPLINE_CURVE_WITH_KNOTS('',3,(#25306,#25307,#25308,#25309,#25310,
#25311,#25312,#25313,#25314,#25315,#25316,#25317,#25318,#25319,#25320,#25321,
#25322,#25323,#25324,#25325,#25326,#25327),.UNSPECIFIED.,.F.,.F.,(4,2,2,
2,2,2,2,2,2,2,4),(0.516725915130786,0.527390969880923,0.571339243451659,
0.615287517022395,0.659234130021226,0.703180743020056,0.747127356018888,
0.791073969017719,0.835022242588455,0.87897051615919,0.889635570909327),
 .UNSPECIFIED.);
#995=B_SPLINE_CURVE_WITH_KNOTS('',3,(#25330,#25331,#25332,#25333),
 .UNSPECIFIED.,.F.,.F.,(4,4),(0.767662411819254,0.784327025837645),
 .UNSPECIFIED.);
#996=B_SPLINE_CURVE_WITH_KNOTS('',3,(#25336,#25337,#25338,#25339,#25340,
#25341,#25342,#25343,#25344,#25345,#25346,#25347,#25348,#25349,#25350,#25351,
#25352,#25353,#25354,#25355,#25356,#25357,#25358),.UNSPECIFIED.,.F.,.F.,
(4,2,2,2,2,3,2,2,2,2,4),(-0.186453873187254,-0.17578960100413,-0.131841711164796,
-0.0878938213254616,-0.0439469106627308,0.,0.0439469106627307,0.0878938213254613,
0.131841711164795,0.17578960100413,0.186453873187382),.UNSPECIFIED.);
#997=B_SPLINE_CURVE_WITH_KNOTS('',3,(#25360,#25361,#25362,#25363,#25364,
#25365,#25366,#25367,#25368,#25369,#25370,#25371,#25372,#25373,#25374,#25375,
#25376,#25377,#25378,#25379,#25380,#25381,#25382),.UNSPECIFIED.,.F.,.F.,
(4,2,2,2,2,3,2,2,2,2,4),(-0.186453873187253,-0.17578960100413,-0.131841711164795,
-0.0878938213254608,-0.0439469106627304,0.,0.0439469106627304,0.0878938213254609,
0.131841711164795,0.17578960100413,0.186453873187382),.UNSPECIFIED.);
#998=B_SPLINE_CURVE_WITH_KNOTS('',3,(#25386,#25387,#25388,#25389,#25390,
#25391,#25392,#25393,#25394,#25395,#25396,#25397,#25398,#25399,#25400,#25401,
#25402,#25403,#25404,#25405,#25406,#25407),.UNSPECIFIED.,.F.,.F.,(4,2,2,
2,2,2,2,2,2,2,4),(0.516725915130786,0.527390969880923,0.571339243451659,
0.615287517022395,0.659234130021226,0.703180743020057,0.747127356018888,
0.791073969017719,0.835022242588455,0.878970516159191,0.889635570909327),
 .UNSPECIFIED.);
#999=B_SPLINE_CURVE_WITH_KNOTS('',3,(#25411,#25412,#25413,#25414),
 .UNSPECIFIED.,.F.,.F.,(4,4),(0.750997797800867,0.767662411819255),
 .UNSPECIFIED.);
#1000=B_SPLINE_CURVE_WITH_KNOTS('',3,(#25415,#25416,#25417,#25418,#25419,
#25420,#25421,#25422,#25423,#25424,#25425,#25426,#25427,#25428,#25429,#25430,
#25431,#25432,#25433,#25434,#25435,#25436),.UNSPECIFIED.,.F.,.F.,(4,2,2,
2,2,2,2,2,2,2,4),(0.516725915130786,0.527390969880923,0.571339243451659,
0.615287517022395,0.659234130021226,0.703180743020057,0.747127356018888,
0.791073969017718,0.835022242588454,0.87897051615919,0.889635570909327),
 .UNSPECIFIED.);
#1001=B_SPLINE_CURVE_WITH_KNOTS('',3,(#25439,#25440,#25441,#25442),
 .UNSPECIFIED.,.F.,.F.,(4,4),(0.767662411819255,0.784327025837643),
 .UNSPECIFIED.);
#1002=B_SPLINE_CURVE_WITH_KNOTS('',3,(#25445,#25446,#25447,#25448,#25449,
#25450,#25451,#25452,#25453,#25454,#25455,#25456,#25457,#25458,#25459,#25460,
#25461,#25462,#25463,#25464,#25465,#25466,#25467),.UNSPECIFIED.,.F.,.F.,
(4,2,2,2,2,3,2,2,2,2,4),(-0.186453873187253,-0.17578960100413,-0.131841711164795,
-0.0878938213254608,-0.0439469106627304,0.,0.0439469106627304,0.0878938213254608,
0.131841711164795,0.17578960100413,0.186453873187381),.UNSPECIFIED.);
#1003=B_SPLINE_CURVE_WITH_KNOTS('',3,(#25469,#25470,#25471,#25472,#25473,
#25474,#25475,#25476,#25477,#25478,#25479,#25480,#25481,#25482,#25483,#25484,
#25485,#25486,#25487,#25488,#25489,#25490,#25491),.UNSPECIFIED.,.F.,.F.,
(4,2,2,2,2,3,2,2,2,2,4),(-0.186453873187253,-0.17578960100413,-0.131841711164796,
-0.0878938213254616,-0.0439469106627308,0.,0.0439469106627304,0.0878938213254609,
0.131841711164795,0.17578960100413,0.186453873187382),.UNSPECIFIED.);
#1004=B_SPLINE_CURVE_WITH_KNOTS('',3,(#25495,#25496,#25497,#25498,#25499,
#25500,#25501,#25502,#25503,#25504,#25505,#25506,#25507,#25508,#25509,#25510,
#25511,#25512,#25513,#25514,#25515,#25516),.UNSPECIFIED.,.F.,.F.,(4,2,2,
2,2,2,2,2,2,2,4),(0.516725915130786,0.527390969880923,0.571339243451659,
0.615287517022395,0.659234130021226,0.703180743020057,0.747127356018888,
0.791073969017719,0.835022242588455,0.878970516159191,0.889635570909328),
 .UNSPECIFIED.);
#1005=B_SPLINE_CURVE_WITH_KNOTS('',3,(#25519,#25520,#25521,#25522),
 .UNSPECIFIED.,.F.,.F.,(4,4),(0.767662411819255,0.784327025837642),
 .UNSPECIFIED.);
#1006=B_SPLINE_CURVE_WITH_KNOTS('',3,(#25526,#25527,#25528,#25529),
 .UNSPECIFIED.,.F.,.F.,(4,4),(0.750997797800867,0.767662411819255),
 .UNSPECIFIED.);
#1007=B_SPLINE_CURVE_WITH_KNOTS('',3,(#25530,#25531,#25532,#25533,#25534,
#25535,#25536,#25537,#25538,#25539,#25540,#25541,#25542,#25543,#25544,#25545,
#25546,#25547,#25548,#25549,#25550,#25551),.UNSPECIFIED.,.F.,.F.,(4,2,2,
2,2,2,2,2,2,2,4),(0.516725915130786,0.527390969880923,0.571339243451659,
0.615287517022395,0.659234130021226,0.703180743020057,0.747127356018888,
0.791073969017719,0.835022242588455,0.878970516159191,0.889635570909327),
 .UNSPECIFIED.);
#1008=B_SPLINE_CURVE_WITH_KNOTS('',3,(#25554,#25555,#25556,#25557,#25558,
#25559,#25560,#25561,#25562,#25563,#25564,#25565,#25566,#25567,#25568,#25569,
#25570,#25571,#25572,#25573,#25574,#25575,#25576),.UNSPECIFIED.,.F.,.F.,
(4,2,2,2,2,3,2,2,2,2,4),(-0.186453873187254,-0.17578960100413,-0.131841711164795,
-0.087893821325461,-0.0439469106627304,0.,0.0439469106627308,0.0878938213254617,
0.131841711164796,0.17578960100413,0.186453873187381),.UNSPECIFIED.);
#1009=B_SPLINE_CURVE_WITH_KNOTS('',3,(#25582,#25583,#25584,#25585,#25586,
#25587,#25588,#25589,#25590,#25591,#25592,#25593,#25594,#25595,#25596,#25597,
#25598,#25599,#25600,#25601,#25602,#25603,#25604),.UNSPECIFIED.,.F.,.F.,
(4,2,2,2,2,3,2,2,2,2,4),(-0.186453873187253,-0.17578960100413,-0.131841711164795,
-0.0878938213254608,-0.0439469106627304,0.,0.0439469106627304,0.0878938213254609,
0.131841711164795,0.17578960100413,0.186453873187381),.UNSPECIFIED.);
#1010=B_SPLINE_CURVE_WITH_KNOTS('',3,(#25612,#25613,#25614,#25615),
 .UNSPECIFIED.,.F.,.F.,(4,4),(0.750997797800867,0.767662411819255),
 .UNSPECIFIED.);
#1011=B_SPLINE_CURVE_WITH_KNOTS('',3,(#25617,#25618,#25619,#25620),
 .UNSPECIFIED.,.F.,.F.,(4,4),(0.767662411819255,0.784327025837643),
 .UNSPECIFIED.);
#1012=B_SPLINE_CURVE_WITH_KNOTS('',3,(#25623,#25624,#25625,#25626,#25627,
#25628,#25629,#25630,#25631,#25632,#25633,#25634,#25635,#25636,#25637,#25638,
#25639,#25640,#25641,#25642,#25643,#25644),.UNSPECIFIED.,.F.,.F.,(4,2,2,
2,2,2,2,2,2,2,4),(0.516725915130786,0.527390969880923,0.571339243451659,
0.615287517022395,0.659234130021226,0.703180743020057,0.747127356018888,
0.791073969017719,0.835022242588455,0.878970516159191,0.889635570909328),
 .UNSPECIFIED.);
#1013=B_SPLINE_CURVE_WITH_KNOTS('',3,(#25648,#25649,#25650,#25651,#25652,
#25653,#25654,#25655,#25656,#25657,#25658,#25659,#25660,#25661,#25662,#25663,
#25664,#25665,#25666,#25667,#25668,#25669),.UNSPECIFIED.,.F.,.F.,(4,2,2,
2,2,2,2,2,2,2,4),(0.516725915130786,0.527390969880923,0.571339243451659,
0.615287517022395,0.659234130021226,0.703180743020057,0.747127356018888,
0.791073969017719,0.835022242588455,0.878970516159191,0.889635570909327),
 .UNSPECIFIED.);
#1014=B_SPLINE_CURVE_WITH_KNOTS('',3,(#25672,#25673,#25674,#25675,#25676,
#25677,#25678,#25679,#25680,#25681,#25682,#25683,#25684,#25685,#25686,#25687,
#25688,#25689,#25690,#25691,#25692,#25693,#25694),.UNSPECIFIED.,.F.,.F.,
(4,2,2,2,2,3,2,2,2,2,4),(-0.186453873187253,-0.17578960100413,-0.131841711164795,
-0.087893821325461,-0.0439469106627306,0.,0.0439469106627304,0.0878938213254609,
0.131841711164795,0.17578960100413,0.186453873187381),.UNSPECIFIED.);
#1015=B_SPLINE_CURVE_WITH_KNOTS('',3,(#25849,#25850,#25851,#25852,#25853,
#25854,#25855,#25856,#25857,#25858),.UNSPECIFIED.,.F.,.F.,(4,3,3,4),(-4.09254174883833,
-3.93292792746001,-2.94969594559501,-2.0651401332781),.UNSPECIFIED.);
#1016=B_SPLINE_CURVE_WITH_KNOTS('',3,(#25861,#25862,#25863,#25864,#25865,
#25866,#25867),.UNSPECIFIED.,.F.,.F.,(4,3,4),(0.,0.983231981865002,1.11419103802958),
 .UNSPECIFIED.);
#1017=B_SPLINE_CURVE_WITH_KNOTS('',3,(#25872,#25873,#25874,#25875,#25876,
#25877,#25878,#25879,#25880,#25881,#25882,#25883,#25884,#25885,#25886,#25887,
#25888,#25889,#25890,#25891,#25892,#25893),.UNSPECIFIED.,.F.,.F.,(4,3,3,
3,3,3,3,4),(-10.3757270560179,-9.83231981865002,-8.84908783678502,-7.86585585492002,
-6.88262387305502,-5.89939189119002,-4.91615990932501,-4.09254174883833),
 .UNSPECIFIED.);
#1018=B_SPLINE_CURVE_WITH_KNOTS('',3,(#25894,#25895,#25896,#25897,#25898,
#25899,#25900,#25901,#25902,#25903,#25904,#25905,#25906,#25907,#25908,#25909,
#25910,#25911,#25912,#25913,#25914,#25915),.UNSPECIFIED.,.F.,.F.,(4,3,3,
3,3,3,3,4),(1.11419103802958,1.96646396373,2.94969594559501,3.93292792746001,
4.91615990932501,5.89939189119001,6.88262387305501,7.39737634520916),
 .UNSPECIFIED.);
#1019=B_SPLINE_CURVE_WITH_KNOTS('',3,(#25920,#25921,#25922,#25923,#25924,
#25925,#25926,#25927,#25928,#25929,#25930,#25931,#25932,#25933,#25934,#25935,
#25936,#25937,#25938,#25939,#25940,#25941),.UNSPECIFIED.,.F.,.F.,(4,3,3,
3,3,3,3,4),(-16.6589123631975,-15.73171170984,-14.748479727975,-13.76524774611,
-12.782015764245,-11.79878378238,-10.815551800515,-10.3757270560179),
 .UNSPECIFIED.);
#1020=B_SPLINE_CURVE_WITH_KNOTS('',3,(#25942,#25943,#25944,#25945,#25946,
#25947,#25948,#25949,#25950,#25951,#25952,#25953,#25954,#25955,#25956,#25957,
#25958,#25959,#25960,#25961,#25962,#25963),.UNSPECIFIED.,.F.,.F.,(4,3,3,
3,3,3,3,4),(7.39737634520916,7.86585585492002,8.84908783678502,9.83231981865002,
10.815551800515,11.79878378238,12.782015764245,13.6805616523888),
 .UNSPECIFIED.);
#1021=B_SPLINE_CURVE_WITH_KNOTS('',3,(#25968,#25969,#25970,#25971,#25972,
#25973,#25974,#25975,#25976,#25977,#25978,#25979,#25980,#25981,#25982,#25983,
#25984,#25985,#25986,#25987,#25988,#25989,#25990,#25991,#25992),
 .UNSPECIFIED.,.F.,.F.,(4,3,3,3,3,3,3,3,4),(-22.9420976703771,-22.6143355828951,
-21.6311036010301,-20.647871619165,-19.6646396373,-18.681407655435,-17.69817567357,
-16.714943691705,-16.6589123631975),.UNSPECIFIED.);
#1022=B_SPLINE_CURVE_WITH_KNOTS('',3,(#25993,#25994,#25995,#25996,#25997,
#25998,#25999,#26000,#26001,#26002,#26003,#26004,#26005,#26006,#26007,#26008,
#26009,#26010,#26011,#26012,#26013,#26014,#26015,#26016,#26017),
 .UNSPECIFIED.,.F.,.F.,(4,3,3,3,3,3,3,3,4),(13.6805616523888,13.76524774611,
14.748479727975,15.73171170984,16.714943691705,17.69817567357,18.681407655435,
19.6646396373,19.9637469595683),.UNSPECIFIED.);
#1023=B_SPLINE_CURVE_WITH_KNOTS('',3,(#26022,#26023,#26024,#26025,#26026,
#26027,#26028,#26029,#26030,#26031,#26032,#26033,#26034,#26035,#26036,#26037,
#26038,#26039,#26040,#26041,#26042,#26043),.UNSPECIFIED.,.F.,.F.,(4,3,3,
3,3,3,3,4),(-29.2252829775567,-28.5137274740851,-27.5304954922201,-26.5472635103551,
-25.5640315284901,-24.5807995466251,-23.5975675647601,-22.9420976703771),
 .UNSPECIFIED.);
#1024=B_SPLINE_CURVE_WITH_KNOTS('',3,(#26044,#26045,#26046,#26047,#26048,
#26049,#26050,#26051,#26052,#26053,#26054,#26055,#26056,#26057,#26058,#26059,
#26060,#26061,#26062,#26063,#26064,#26065),.UNSPECIFIED.,.F.,.F.,(4,3,3,
3,3,3,3,4),(19.9637469595683,20.647871619165,21.63110360103,22.614335582895,
23.59756756476,24.580799546625,25.5640315284901,26.2469322667479),
 .UNSPECIFIED.);
#1025=B_SPLINE_CURVE_WITH_KNOTS('',3,(#26070,#26071,#26072,#26073,#26074,
#26075,#26076,#26077,#26078,#26079,#26080,#26081,#26082,#26083,#26084,#26085,
#26086,#26087,#26088,#26089,#26090,#26091,#26092,#26093,#26094),
 .UNSPECIFIED.,.F.,.F.,(4,3,3,3,3,3,3,3,4),(-35.5084682847363,-35.3963513471401,
-34.4131193652751,-33.4298873834101,-32.4466554015451,-31.4634234196801,
-30.4801914378151,-29.4969594559501,-29.2252829775567),.UNSPECIFIED.);
#1026=B_SPLINE_CURVE_WITH_KNOTS('',3,(#26095,#26096,#26097,#26098,#26099,
#26100,#26101,#26102,#26103,#26104,#26105,#26106,#26107,#26108,#26109,#26110,
#26111,#26112,#26113,#26114,#26115,#26116,#26117,#26118,#26119),
 .UNSPECIFIED.,.F.,.F.,(4,3,3,3,3,3,3,3,4),(26.2469322667479,26.547263510355,
27.5304954922201,28.5137274740851,29.4969594559501,30.4801914378151,31.4634234196801,
32.4466554015451,32.5301175739275),.UNSPECIFIED.);
#1027=B_SPLINE_CURVE_WITH_KNOTS('',3,(#26125,#26126,#26127,#26128),
 .UNSPECIFIED.,.F.,.F.,(4,4),(47.1238898038469,47.8963286785676),
 .UNSPECIFIED.);
#1028=B_SPLINE_CURVE_WITH_KNOTS('',3,(#26134,#26135,#26136,#26137,#26138,
#26139,#26140,#26141,#26142,#26143,#26144),.UNSPECIFIED.,.F.,.F.,(4,1,1,
1,1,1,1,1,4),(40.8407044966673,41.1123809750607,42.0956129569257,43.0788449387907,
44.0620769206557,45.0453089025207,46.0285408843857,47.0117728662507,47.1238898038469),
 .UNSPECIFIED.);
#1029=B_SPLINE_CURVE_WITH_KNOTS('',3,(#26147,#26148,#26149,#26150,#26151,
#26152,#26153,#26154,#26155),.UNSPECIFIED.,.F.,.F.,(4,1,1,1,1,1,4),(40.8407044966673,
41.7404743061498,42.7237062880148,43.7069382698798,44.6901702517448,45.6734022336098,
46.6566342154749),.UNSPECIFIED.);
#1030=B_SPLINE_CURVE_WITH_KNOTS('',3,(#26160,#26161,#26162,#26163,#26164,
#26165,#26166,#26167,#26168,#26169),.UNSPECIFIED.,.F.,.F.,(4,1,1,1,1,1,
1,4),(34.5575191894877,35.2129890838707,36.1962210657357,37.1794530476007,
38.1626850294657,39.1459170113307,40.1291489931957,40.8407044966673),
 .UNSPECIFIED.);
#1031=B_SPLINE_CURVE_WITH_KNOTS('',3,(#26170,#26171,#26172,#26173,#26174,
#26175,#26176,#26177,#26178,#26179,#26180),.UNSPECIFIED.,.F.,.F.,(4,1,1,
1,1,1,1,1,4),(34.5575191894877,34.8578504330948,35.8410824149598,36.8243143968248,
37.8075463786898,38.7907783605548,39.7740103424198,40.7572423242848,40.8407044966673),
 .UNSPECIFIED.);
#1032=B_SPLINE_CURVE_WITH_KNOTS('',3,(#26185,#26186,#26187,#26188,#26189,
#26190,#26191,#26192,#26193,#26194,#26195),.UNSPECIFIED.,.F.,.F.,(4,1,1,
1,1,1,1,1,4),(28.2743338823081,28.3303652108157,29.3135971926807,30.2968291745457,
31.2800611564107,32.2632931382757,33.2465251201407,34.2297571020057,34.5575191894877),
 .UNSPECIFIED.);
#1033=B_SPLINE_CURVE_WITH_KNOTS('',3,(#26196,#26197,#26198,#26199,#26200,
#26201,#26202,#26203,#26204,#26205),.UNSPECIFIED.,.F.,.F.,(4,1,1,1,1,1,
1,4),(28.2743338823081,28.9584585419048,29.9416905237698,30.9249225056348,
31.9081544874998,32.8913864693648,33.8746184512298,34.5575191894877),
 .UNSPECIFIED.);
#1034=B_SPLINE_CURVE_WITH_KNOTS('',3,(#26210,#26211,#26212,#26213,#26214,
#26215,#26216,#26217,#26218,#26219),.UNSPECIFIED.,.F.,.F.,(4,1,1,1,1,1,
1,4),(21.9911485751285,22.4309733196257,23.4142053014907,24.3974372833557,
25.3806692652207,26.3639012470857,27.3471332289507,28.2743338823081),
 .UNSPECIFIED.);
#1035=B_SPLINE_CURVE_WITH_KNOTS('',3,(#26220,#26221,#26222,#26223,#26224,
#26225,#26226,#26227,#26228,#26229,#26230),.UNSPECIFIED.,.F.,.F.,(4,1,1,
1,1,1,1,1,4),(21.9911485751285,22.0758346688498,23.0590666507148,24.0422986325798,
25.0255306144448,26.0087625963098,26.9919945781748,27.9752265600398,28.2743338823081),
 .UNSPECIFIED.);
#1036=B_SPLINE_CURVE_WITH_KNOTS('',3,(#26235,#26236,#26237,#26238,#26239,
#26240,#26241,#26242,#26243,#26244),.UNSPECIFIED.,.F.,.F.,(4,1,1,1,1,1,
1,4),(15.707963267949,16.5315814284356,17.5148134103006,18.4980453921656,
19.4812773740306,20.4645093558957,21.4477413377607,21.9911485751285),
 .UNSPECIFIED.);
#1037=B_SPLINE_CURVE_WITH_KNOTS('',3,(#26245,#26246,#26247,#26248,#26249,
#26250,#26251,#26252,#26253,#26254),.UNSPECIFIED.,.F.,.F.,(4,1,1,1,1,1,
1,4),(15.707963267949,16.1764427776598,17.1596747595248,18.1429067413898,
19.1261387232548,20.1093707051198,21.0926026869848,21.9911485751285),
 .UNSPECIFIED.);
#1038=B_SPLINE_CURVE_WITH_KNOTS('',3,(#26257,#26258,#26259,#26260,#26261,
#26262,#26263,#26264,#26265,#26266,#26267,#26268,#26269,#26270,#26271,#26272,
#26273,#26274,#26275,#26276,#26277,#26278,#26279,#26280,#26281,#26282,#26283,
#26284,#26285,#26286,#26287,#26288,#26289,#26290,#26291,#26292,#26293,#26294,
#26295,#26296,#26297,#26298,#26299,#26300,#26301,#26302,#26303,#26304,#26305,
#26306,#26307,#26308),.UNSPECIFIED.,.F.,.F.,(4,3,3,3,3,3,3,3,3,3,3,3,3,
3,3,3,3,4),(-0.366397579005844,-0.350753953906653,-0.330463017686532,-0.315435531128199,
-0.287643881494464,-0.272924732924834,-0.237814891323476,-0.221795460451242,
-0.207726041133023,-0.184571159408416,-0.160894855415823,-0.147419681563097,
-0.13576580392061,-0.101824352940458,-0.0769585672558313,-0.0671142413070353,
-0.0286195295740189,0.),.UNSPECIFIED.);
#1039=B_SPLINE_CURVE_WITH_KNOTS('',3,(#26313,#26314,#26315,#26316,#26317,
#26318,#26319,#26320,#26321,#26322,#26323,#26324,#26325,#26326,#26327,#26328,
#26329,#26330,#26331,#26332,#26333,#26334,#26335,#26336,#26337,#26338,#26339,
#26340,#26341,#26342,#26343,#26344,#26345,#26346,#26347,#26348,#26349,#26350,
#26351,#26352,#26353,#26354,#26355,#26356,#26357,#26358,#26359,#26360,#26361,
#26362,#26363,#26364,#26365,#26366,#26367),.UNSPECIFIED.,.F.,.F.,(4,3,3,
3,3,3,3,3,3,3,3,3,3,3,3,3,3,3,4),(-0.364629307890667,-0.345405509511423,
-0.316109491299348,-0.303964239439482,-0.281709554317525,-0.264921543558191,
-0.252375276770721,-0.215944087132777,-0.198753901855764,-0.18596810420685,
-0.163689794923203,-0.143278793185558,-0.127728424538677,-0.117434610457182,
-0.0880759578428862,-0.0702652452140735,-0.0601818930641948,-0.0277041096514565,
0.),.UNSPECIFIED.);
#1040=B_SPLINE_CURVE_WITH_KNOTS('',3,(#26536,#26537,#26538,#26539,#26540,
#26541,#26542,#26543,#26544,#26545,#26546,#26547,#26548),.UNSPECIFIED.,
 .F.,.F.,(4,3,3,3,4),(32.5301175739275,33.4298873834101,34.4131193652751,
35.3963513471401,36.280907159457),.UNSPECIFIED.);
#1041=B_SPLINE_CURVE_WITH_KNOTS('',3,(#26550,#26551,#26552,#26553,#26554,
#26555,#26556,#26557,#26558,#26559,#26560,#26561,#26562,#26563,#26564,#26565,
#26566,#26567,#26568,#26569,#26570,#26571,#26572,#26573,#26574,#26575,#26576,
#26577,#26578,#26579,#26580,#26581,#26582,#26583,#26584,#26585,#26586,#26587,
#26588,#26589,#26590,#26591,#26592,#26593,#26594,#26595,#26596,#26597,#26598,
#26599,#26600,#26601),.UNSPECIFIED.,.F.,.F.,(4,3,3,3,3,3,3,3,3,3,3,3,3,
3,3,3,3,4),(-0.366397579005851,-0.350753953906661,-0.330463024735024,-0.315435543259483,
-0.287644877982493,-0.272925011059114,-0.237815179368718,-0.221795848896316,
-0.207726060922694,-0.184571159408424,-0.160894850055595,-0.147419600331868,
-0.135765787605129,-0.101824340703847,-0.0769585196865098,-0.0671141722159687,
-0.0286194368321035,0.),.UNSPECIFIED.);
#1042=B_SPLINE_CURVE_WITH_KNOTS('',3,(#26602,#26603,#26604,#26605,#26606,
#26607,#26608,#26609,#26610),.UNSPECIFIED.,.F.,.F.,(4,1,1,1,1,1,4),(10.3757270560179,
11.2602828683348,12.2435148501998,13.2267468320648,14.2099788139298,15.1932107957948,
15.707963267949),.UNSPECIFIED.);
#1043=B_SPLINE_CURVE_WITH_KNOTS('',3,(#26616,#26617,#26618,#26619,#26620,
#26621,#26622,#26623,#26624,#26625,#26626,#26627,#26628,#26629,#26630,#26631,
#26632,#26633,#26634,#26635,#26636,#26637,#26638,#26639,#26640,#26641,#26642,
#26643,#26644,#26645,#26646,#26647,#26648,#26649,#26650,#26651,#26652,#26653,
#26654,#26655,#26656,#26657,#26658,#26659,#26660,#26661,#26662,#26663,#26664,
#26665,#26666,#26667,#26668,#26669,#26670),.UNSPECIFIED.,.F.,.F.,(4,3,3,
3,3,3,3,3,3,3,3,3,3,3,3,3,3,3,4),(-0.364629307890684,-0.345405509511438,
-0.316109466616483,-0.303964180518109,-0.28170938055002,-0.264921036000774,
-0.252375151029453,-0.215943930999405,-0.198753706254068,-0.185968021399695,
-0.163689794923211,-0.143278681804942,-0.127728193637607,-0.117434275921994,
-0.0880757069414953,-0.070264744543059,-0.0601814248546799,-0.0277037327266843,
0.),.UNSPECIFIED.);
#1044=B_SPLINE_CURVE_WITH_KNOTS('',3,(#26673,#26674,#26675,#26676,#26677,
#26678,#26679,#26680),.UNSPECIFIED.,.F.,.F.,(4,1,1,1,1,4),(11.6154215191106,
12.5986535009756,13.5818854828406,14.5651174647056,15.5483494465706,15.707963267949),
 .UNSPECIFIED.);
#1045=B_SPLINE_CURVE_WITH_KNOTS('',3,(#26849,#26850,#26851,#26852,#26853,
#26854,#26855,#26856,#26857,#26858),.UNSPECIFIED.,.F.,.F.,(4,3,3,4),(-38.3460472927351,
-37.3628153108701,-36.3795833290051,-35.5084682847363),.UNSPECIFIED.);
#1046=B_SPLINE_CURVE_WITH_KNOTS('',3,(#26914,#26915,#26916,#26917,#26918,
#26919,#26920,#26921,#26922,#26923),.UNSPECIFIED.,.F.,.F.,(4,3,3,4),(-4.09293042013064,
-3.99248307740831,-2.99436230805624,-2.06863817490914),.UNSPECIFIED.);
#1047=B_SPLINE_CURVE_WITH_KNOTS('',3,(#26926,#26927,#26928,#26929,#26930,
#26931,#26932),.UNSPECIFIED.,.F.,.F.,(4,3,4),(0.,0.998120769352068,1.11730040836818),
 .UNSPECIFIED.);
#1048=B_SPLINE_CURVE_WITH_KNOTS('',3,(#26937,#26938,#26939,#26940,#26941,
#26942,#26943,#26944,#26945,#26946,#26947,#26948,#26949,#26950,#26951,#26952,
#26953,#26954,#26955,#26956,#26957,#26958),.UNSPECIFIED.,.F.,.F.,(4,3,3,
3,3,3,3,4),(-10.3761157273103,-9.98120769352079,-8.98308692416871,-7.98496615481663,
-6.98684538546455,-5.98872461611248,-4.99060384676039,-4.09293042013064),
 .UNSPECIFIED.);
#1049=B_SPLINE_CURVE_WITH_KNOTS('',3,(#26959,#26960,#26961,#26962,#26963,
#26964,#26965,#26966,#26967,#26968,#26969,#26970,#26971,#26972,#26973,#26974,
#26975,#26976,#26977,#26978,#26979,#26980),.UNSPECIFIED.,.F.,.F.,(4,3,3,
3,3,3,3,4),(1.11730040836818,1.99624153870415,2.99436230805623,3.99248307740831,
4.99060384676039,5.98872461611247,6.98684538546454,7.40048571554779),
 .UNSPECIFIED.);
#1050=B_SPLINE_CURVE_WITH_KNOTS('',3,(#26985,#26986,#26987,#26988,#26989,
#26990,#26991,#26992,#26993,#26994,#26995,#26996,#26997,#26998,#26999,#27000,
#27001,#27002,#27003,#27004,#27005,#27006),.UNSPECIFIED.,.F.,.F.,(4,3,3,
3,3,3,3,4),(-16.6593010344898,-15.9699323096333,-14.9718115402812,-13.9736907709291,
-12.975570001577,-11.9774492322249,-10.9793284628729,-10.3761157273103),
 .UNSPECIFIED.);
#1051=B_SPLINE_CURVE_WITH_KNOTS('',3,(#27007,#27008,#27009,#27010,#27011,
#27012,#27013,#27014,#27015,#27016,#27017,#27018,#27019,#27020,#27021,#27022,
#27023,#27024,#27025,#27026,#27027,#27028),.UNSPECIFIED.,.F.,.F.,(4,3,3,
3,3,3,3,4),(7.40048571554779,7.98496615481663,8.9830869241687,9.98120769352078,
10.9793284628729,11.9774492322249,12.975570001577,13.6836710227274),
 .UNSPECIFIED.);
#1052=B_SPLINE_CURVE_WITH_KNOTS('',3,(#27033,#27034,#27035,#27036,#27037,
#27038,#27039,#27040,#27041,#27042,#27043,#27044,#27045,#27046,#27047,#27048,
#27049,#27050,#27051,#27052,#27053,#27054),.UNSPECIFIED.,.F.,.F.,(4,3,3,
3,3,3,3,4),(-22.9424863416694,-21.9586569257457,-20.9605361563937,-19.9624153870416,
-18.9642946176895,-17.9661738483374,-16.9680530789853,-16.6593010344898),
 .UNSPECIFIED.);
#1053=B_SPLINE_CURVE_WITH_KNOTS('',3,(#27055,#27056,#27057,#27058,#27059,
#27060,#27061,#27062,#27063,#27064,#27065,#27066,#27067,#27068,#27069,#27070,
#27071,#27072,#27073,#27074,#27075,#27076,#27077,#27078,#27079),
 .UNSPECIFIED.,.F.,.F.,(4,3,3,3,3,3,3,3,4),(13.6836710227274,13.9736907709291,
14.9718115402812,15.9699323096333,16.9680530789853,17.9661738483374,18.9642946176895,
19.9624153870416,19.966856329907),.UNSPECIFIED.);
#1054=B_SPLINE_CURVE_WITH_KNOTS('',3,(#27084,#27085,#27086,#27087,#27088,
#27089,#27090,#27091,#27092,#27093,#27094,#27095,#27096,#27097,#27098,#27099,
#27100,#27101,#27102,#27103,#27104,#27105,#27106,#27107,#27108),
 .UNSPECIFIED.,.F.,.F.,(4,3,3,3,3,3,3,3,4),(-29.225671648849,-28.9455023112103,
-27.9473815418582,-26.9492607725061,-25.9511400031541,-24.953019233802,
-23.9548984644499,-22.9567776950978,-22.9424863416694),.UNSPECIFIED.);
#1055=B_SPLINE_CURVE_WITH_KNOTS('',3,(#27109,#27110,#27111,#27112,#27113,
#27114,#27115,#27116,#27117,#27118,#27119,#27120,#27121,#27122,#27123,#27124,
#27125,#27126,#27127,#27128,#27129,#27130),.UNSPECIFIED.,.F.,.F.,(4,3,3,
3,3,3,3,4),(19.966856329907,20.9605361563937,21.9586569257457,22.9567776950978,
23.9548984644499,24.953019233802,25.9511400031541,26.2500416370865),
 .UNSPECIFIED.);
#1056=B_SPLINE_CURVE_WITH_KNOTS('',3,(#27135,#27136,#27137,#27138,#27139,
#27140,#27141,#27142,#27143,#27144,#27145,#27146,#27147,#27148,#27149,#27150,
#27151,#27152,#27153,#27154,#27155,#27156),.UNSPECIFIED.,.F.,.F.,(4,3,3,
3,3,3,3,4),(-35.5088569560286,-34.9342269273228,-33.9361061579707,-32.9379853886186,
-31.9398646192665,-30.9417438499144,-29.9436230805624,-29.225671648849),
 .UNSPECIFIED.);
#1057=B_SPLINE_CURVE_WITH_KNOTS('',3,(#27157,#27158,#27159,#27160,#27161,
#27162,#27163,#27164,#27165,#27166,#27167,#27168,#27169,#27170,#27171,#27172,
#27173,#27174,#27175,#27176,#27177,#27178),.UNSPECIFIED.,.F.,.F.,(4,3,3,
3,3,3,3,4),(26.2500416370865,26.9492607725061,27.9473815418582,28.9455023112103,
29.9436230805624,30.9417438499144,31.9398646192665,32.5332269442662),
 .UNSPECIFIED.);
#1058=B_SPLINE_CURVE_WITH_KNOTS('',3,(#27183,#27184,#27185,#27186,#27187,
#27188,#27189,#27190,#27191,#27192,#27193,#27194,#27195,#27196,#27197,#27198,
#27199,#27200,#27201,#27202,#27203,#27204),.UNSPECIFIED.,.F.,.F.,(4,3,3,
3,3,3,3,4),(-41.7920422632082,-40.9229515434352,-39.9248307740831,-38.9267100047311,
-37.928589235379,-36.9304684660269,-35.9323476966748,-35.5088569560286),
 .UNSPECIFIED.);
#1059=B_SPLINE_CURVE_WITH_KNOTS('',3,(#27205,#27206,#27207,#27208,#27209,
#27210,#27211,#27212,#27213,#27214,#27215,#27216,#27217,#27218,#27219,#27220,
#27221,#27222,#27223,#27224,#27225,#27226),.UNSPECIFIED.,.F.,.F.,(4,3,3,
3,3,3,3,4),(32.5332269442662,32.9379853886186,33.9361061579707,34.9342269273227,
35.9323476966748,36.9304684660269,37.928589235379,38.8164122514457),
 .UNSPECIFIED.);
#1060=B_SPLINE_CURVE_WITH_KNOTS('',3,(#27231,#27232,#27233,#27234,#27235,
#27236,#27237,#27238,#27239,#27240,#27241,#27242,#27243,#27244,#27245,#27246,
#27247,#27248,#27249,#27250,#27251,#27252,#27253,#27254,#27255),
 .UNSPECIFIED.,.F.,.F.,(4,3,3,3,3,3,3,3,4),(-48.0752275703878,-47.9097969288998,
-46.9116761595477,-45.9135553901956,-44.9154346208435,-43.9173138514915,
-42.9191930821394,-41.9210723127873,-41.7920422632082),.UNSPECIFIED.);
#1061=B_SPLINE_CURVE_WITH_KNOTS('',3,(#27256,#27257,#27258,#27259,#27260,
#27261,#27262,#27263,#27264,#27265,#27266,#27267,#27268,#27269,#27270,#27271,
#27272,#27273,#27274,#27275,#27276,#27277,#27278,#27279,#27280),
 .UNSPECIFIED.,.F.,.F.,(4,3,3,3,3,3,3,3,4),(38.8164122514457,38.9267100047311,
39.9248307740831,40.9229515434352,41.9210723127873,42.9191930821394,43.9173138514915,
44.9154346208435,45.0995975586253),.UNSPECIFIED.);
#1062=B_SPLINE_CURVE_WITH_KNOTS('',3,(#27285,#27286,#27287,#27288,#27289,
#27290,#27291,#27292,#27293,#27294,#27295,#27296,#27297,#27298,#27299,#27300,
#27301,#27302,#27303,#27304,#27305,#27306),.UNSPECIFIED.,.F.,.F.,(4,3,3,
3,3,3,3,4),(-54.3584128775674,-53.8985215450123,-52.9004007756602,-51.9022800063081,
-50.904159236956,-49.9060384676039,-48.9079176982519,-48.0752275703878),
 .UNSPECIFIED.);
#1063=B_SPLINE_CURVE_WITH_KNOTS('',3,(#27307,#27308,#27309,#27310,#27311,
#27312,#27313,#27314,#27315,#27316,#27317,#27318,#27319,#27320,#27321,#27322,
#27323,#27324,#27325,#27326,#27327,#27328),.UNSPECIFIED.,.F.,.F.,(4,3,3,
3,3,3,3,4),(45.0995975586253,45.9135553901956,46.9116761595477,47.9097969288998,
48.9079176982519,49.9060384676039,50.904159236956,51.3827828658049),
 .UNSPECIFIED.);
#1064=B_SPLINE_CURVE_WITH_KNOTS('',3,(#27333,#27334,#27335,#27336,#27337,
#27338,#27339,#27340,#27341,#27342,#27343,#27344,#27345,#27346,#27347,#27348,
#27349,#27350,#27351,#27352,#27353,#27354),.UNSPECIFIED.,.F.,.F.,(4,3,3,
3,3,3,3,4),(-60.6415981847469,-59.8872461611247,-58.8891253917727,-57.8910046224206,
-56.8928838530685,-55.8947630837164,-54.8966423143643,-54.3584128775674),
 .UNSPECIFIED.);
#1065=B_SPLINE_CURVE_WITH_KNOTS('',3,(#27355,#27356,#27357,#27358,#27359,
#27360,#27361,#27362,#27363,#27364,#27365,#27366,#27367,#27368,#27369,#27370,
#27371,#27372,#27373,#27374,#27375,#27376),.UNSPECIFIED.,.F.,.F.,(4,3,3,
3,3,3,3,4),(51.3827828658049,51.9022800063081,52.9004007756602,53.8985215450123,
54.8966423143643,55.8947630837164,56.8928838530685,57.6659681729845),
 .UNSPECIFIED.);
#1066=B_SPLINE_CURVE_WITH_KNOTS('',3,(#27381,#27382,#27383,#27384,#27385,
#27386,#27387,#27388,#27389,#27390,#27391,#27392,#27393,#27394,#27395,#27396,
#27397,#27398,#27399,#27400,#27401,#27402,#27403,#27404,#27405),
 .UNSPECIFIED.,.F.,.F.,(4,3,3,3,3,3,3,3,4),(-66.9247834919266,-66.8740915465893,
-65.8759707772372,-64.8778500078851,-63.879729238533,-62.881608469181,-61.8834876998289,
-60.8853669304768,-60.6415981847469),.UNSPECIFIED.);
#1067=B_SPLINE_CURVE_WITH_KNOTS('',3,(#27406,#27407,#27408,#27409,#27410,
#27411,#27412,#27413,#27414,#27415,#27416,#27417,#27418,#27419,#27420,#27421,
#27422,#27423,#27424,#27425,#27426,#27427,#27428,#27429,#27430),
 .UNSPECIFIED.,.F.,.F.,(4,3,3,3,3,3,3,3,4),(57.6659681729845,57.8910046224206,
58.8891253917727,59.8872461611247,60.8853669304768,61.8834876998289,62.881608469181,
63.8797292385331,63.9491534801641),.UNSPECIFIED.);
#1068=B_SPLINE_CURVE_WITH_KNOTS('',3,(#27435,#27436,#27437,#27438,#27439,
#27440,#27441,#27442,#27443,#27444,#27445,#27446,#27447,#27448,#27449,#27450,
#27451,#27452,#27453,#27454,#27455,#27456),.UNSPECIFIED.,.F.,.F.,(4,3,3,
3,3,3,3,4),(-73.2079687991062,-72.8628161627017,-71.8646953933497,-70.8665746239976,
-69.8684538546455,-68.8703330852934,-67.8722123159413,-66.9247834919266),
 .UNSPECIFIED.);
#1069=B_SPLINE_CURVE_WITH_KNOTS('',3,(#27457,#27458,#27459,#27460,#27461,
#27462,#27463,#27464,#27465,#27466,#27467,#27468,#27469,#27470,#27471,#27472,
#27473,#27474,#27475,#27476,#27477,#27478),.UNSPECIFIED.,.F.,.F.,(4,3,3,
3,3,3,3,4),(63.9491534801641,64.8778500078851,65.8759707772372,66.8740915465893,
67.8722123159414,68.8703330852934,69.8684538546455,70.2323387873437),
 .UNSPECIFIED.);
#1070=B_SPLINE_CURVE_WITH_KNOTS('',3,(#27483,#27484,#27485,#27486,#27487,
#27488,#27489,#27490,#27491,#27492,#27493,#27494,#27495,#27496,#27497,#27498,
#27499,#27500,#27501,#27502,#27503,#27504),.UNSPECIFIED.,.F.,.F.,(4,3,3,
3,3,3,3,4),(-79.4911541062857,-78.8515407788142,-77.8534200094622,-76.8552992401101,
-75.857178470758,-74.8590577014059,-73.8609369320538,-73.2079687991062),
 .UNSPECIFIED.);
#1071=B_SPLINE_CURVE_WITH_KNOTS('',3,(#27505,#27506,#27507,#27508,#27509,
#27510,#27511,#27512,#27513,#27514,#27515,#27516,#27517,#27518,#27519,#27520,
#27521,#27522,#27523,#27524,#27525,#27526),.UNSPECIFIED.,.F.,.F.,(4,3,3,
3,3,3,3,4),(70.2323387873437,70.8665746239976,71.8646953933497,72.8628161627017,
73.8609369320538,74.8590577014059,75.857178470758,76.5155240945233),
 .UNSPECIFIED.);
#1072=B_SPLINE_CURVE_WITH_KNOTS('',3,(#27531,#27532,#27533,#27534,#27535,
#27536,#27537,#27538,#27539,#27540,#27541,#27542,#27543,#27544,#27545,#27546,
#27547,#27548,#27549,#27550,#27551,#27552),.UNSPECIFIED.,.F.,.F.,(4,3,3,
3,3,3,3,4),(-85.7743394134653,-84.8402653949267,-83.8421446255746,-82.8440238562225,
-81.8459030868705,-80.8477823175184,-79.8496615481663,-79.4911541062857),
 .UNSPECIFIED.);
#1073=B_SPLINE_CURVE_WITH_KNOTS('',3,(#27553,#27554,#27555,#27556,#27557,
#27558,#27559,#27560,#27561,#27562,#27563,#27564,#27565,#27566,#27567,#27568,
#27569,#27570,#27571,#27572,#27573,#27574),.UNSPECIFIED.,.F.,.F.,(4,3,3,
3,3,3,3,4),(76.5155240945233,76.8552992401101,77.8534200094622,78.8515407788142,
79.8496615481663,80.8477823175184,81.8459030868705,82.7987094017029),
 .UNSPECIFIED.);
#1074=B_SPLINE_CURVE_WITH_KNOTS('',3,(#27579,#27580,#27581,#27582,#27583,
#27584,#27585,#27586,#27587,#27588,#27589,#27590,#27591,#27592,#27593,#27594,
#27595,#27596,#27597,#27598,#27599,#27600,#27601,#27602,#27603),
 .UNSPECIFIED.,.F.,.F.,(4,3,3,3,3,3,3,3,4),(-92.0575247206449,-91.8271107803912,
-90.8289900110392,-89.8308692416871,-88.832748472335,-87.8346277029829,
-86.8365069336308,-85.8383861642788,-85.7743394134653),.UNSPECIFIED.);
#1075=B_SPLINE_CURVE_WITH_KNOTS('',3,(#27604,#27605,#27606,#27607,#27608,
#27609,#27610,#27611,#27612,#27613,#27614,#27615,#27616,#27617,#27618,#27619,
#27620,#27621,#27622,#27623,#27624,#27625,#27626,#27627,#27628),
 .UNSPECIFIED.,.F.,.F.,(4,3,3,3,3,3,3,3,4),(82.7987094017029,82.8440238562225,
83.8421446255746,84.8402653949267,85.8383861642788,86.8365069336308,87.834627702983,
88.832748472335,89.0818947088825),.UNSPECIFIED.);
#1076=B_SPLINE_CURVE_WITH_KNOTS('',3,(#27633,#27634,#27635,#27636,#27637,
#27638,#27639,#27640,#27641,#27642,#27643,#27644,#27645,#27646,#27647,#27648,
#27649,#27650,#27651,#27652,#27653,#27654),.UNSPECIFIED.,.F.,.F.,(4,3,3,
3,3,3,3,4),(-98.3407100278245,-97.8158353965037,-96.8177146271516,-95.8195938577995,
-94.8214730884475,-93.8233523190954,-92.8252315497433,-92.0575247206449),
 .UNSPECIFIED.);
#1077=B_SPLINE_CURVE_WITH_KNOTS('',3,(#27655,#27656,#27657,#27658,#27659,
#27660,#27661,#27662,#27663,#27664,#27665,#27666,#27667,#27668,#27669,#27670,
#27671,#27672,#27673,#27674,#27675,#27676),.UNSPECIFIED.,.F.,.F.,(4,3,3,
3,3,3,3,4),(89.0818947088825,89.8308692416871,90.8289900110392,91.8271107803912,
92.8252315497433,93.8233523190954,94.8214730884475,95.3650800160621),
 .UNSPECIFIED.);
#1078=B_SPLINE_CURVE_WITH_KNOTS('',3,(#27681,#27682,#27683,#27684,#27685,
#27686,#27687,#27688,#27689,#27690,#27691,#27692,#27693,#27694,#27695,#27696,
#27697,#27698,#27699,#27700,#27701,#27702),.UNSPECIFIED.,.F.,.F.,(4,3,3,
3,3,3,3,4),(-104.623895335004,-103.804560012616,-102.806439243264,-101.808318473912,
-100.81019770456,-99.8120769352079,-98.8139561658558,-98.3407100278245),
 .UNSPECIFIED.);
#1079=B_SPLINE_CURVE_WITH_KNOTS('',3,(#27703,#27704,#27705,#27706,#27707,
#27708,#27709,#27710,#27711,#27712,#27713,#27714,#27715,#27716,#27717,#27718,
#27719,#27720,#27721,#27722,#27723,#27724),.UNSPECIFIED.,.F.,.F.,(4,3,3,
3,3,3,3,4),(95.3650800160621,95.8195938577996,96.8177146271516,97.8158353965037,
98.8139561658558,99.8120769352079,100.81019770456,101.648265323242),
 .UNSPECIFIED.);
#1080=B_SPLINE_CURVE_WITH_KNOTS('',3,(#27729,#27730,#27731,#27732,#27733,
#27734,#27735,#27736,#27737,#27738,#27739,#27740,#27741,#27742,#27743,#27744,
#27745,#27746,#27747,#27748,#27749,#27750,#27751,#27752,#27753),
 .UNSPECIFIED.,.F.,.F.,(4,3,3,3,3,3,3,3,4),(-110.907080642184,-110.791405398081,
-109.793284628729,-108.795163859377,-107.797043090025,-106.798922320672,
-105.80080155132,-104.802680781968,-104.623895335004),.UNSPECIFIED.);
#1081=B_SPLINE_CURVE_WITH_KNOTS('',3,(#27754,#27755,#27756,#27757,#27758,
#27759,#27760,#27761,#27762,#27763,#27764,#27765,#27766,#27767,#27768,#27769,
#27770,#27771,#27772,#27773,#27774,#27775,#27776,#27777,#27778),
 .UNSPECIFIED.,.F.,.F.,(4,3,3,3,3,3,3,3,4),(101.648265323242,101.808318473912,
102.806439243264,103.804560012616,104.802680781968,105.80080155132,106.798922320672,
107.797043090025,107.931450630421),.UNSPECIFIED.);
#1082=B_SPLINE_CURVE_WITH_KNOTS('',3,(#27783,#27784,#27785,#27786,#27787,
#27788,#27789,#27790,#27791,#27792,#27793,#27794,#27795,#27796,#27797,#27798,
#27799,#27800,#27801,#27802,#27803,#27804),.UNSPECIFIED.,.F.,.F.,(4,3,3,
3,3,3,3,4),(-117.190265949363,-116.780130014193,-115.782009244841,-114.783888475489,
-113.785767706137,-112.787646936785,-111.789526167433,-110.907080642184),
 .UNSPECIFIED.);
#1083=B_SPLINE_CURVE_WITH_KNOTS('',3,(#27805,#27806,#27807,#27808,#27809,
#27810,#27811,#27812,#27813,#27814,#27815,#27816,#27817,#27818,#27819,#27820,
#27821,#27822,#27823,#27824,#27825,#27826),.UNSPECIFIED.,.F.,.F.,(4,3,3,
3,3,3,3,4),(107.931450630421,108.795163859377,109.793284628729,110.791405398081,
111.789526167433,112.787646936785,113.785767706137,114.214635937601),
 .UNSPECIFIED.);
#1084=B_SPLINE_CURVE_WITH_KNOTS('',3,(#27831,#27832,#27833,#27834,#27835,
#27836,#27837,#27838,#27839,#27840,#27841,#27842,#27843,#27844,#27845,#27846,
#27847,#27848,#27849,#27850,#27851,#27852),.UNSPECIFIED.,.F.,.F.,(4,3,3,
3,3,3,3,4),(-123.473451256543,-122.768854630306,-121.770733860954,-120.772613091602,
-119.774492322249,-118.776371552897,-117.778250783545,-117.190265949363),
 .UNSPECIFIED.);
#1085=B_SPLINE_CURVE_WITH_KNOTS('',3,(#27853,#27854,#27855,#27856,#27857,
#27858,#27859,#27860,#27861,#27862,#27863,#27864,#27865,#27866,#27867,#27868,
#27869,#27870,#27871,#27872,#27873,#27874),.UNSPECIFIED.,.F.,.F.,(4,3,3,
3,3,3,3,4),(114.214635937601,114.783888475489,115.782009244841,116.780130014193,
117.778250783545,118.776371552897,119.774492322249,120.49782124478),
 .UNSPECIFIED.);
#1086=B_SPLINE_CURVE_WITH_KNOTS('',3,(#27879,#27880,#27881,#27882,#27883,
#27884,#27885,#27886,#27887,#27888,#27889,#27890,#27891,#27892,#27893,#27894,
#27895,#27896,#27897,#27898,#27899,#27900),.UNSPECIFIED.,.F.,.F.,(4,3,3,
3,3,3,3,4),(-129.756636563722,-128.757579246418,-127.759458477066,-126.761337707714,
-125.763216938362,-124.76509616901,-123.766975399658,-123.473451256543),
 .UNSPECIFIED.);
#1087=B_SPLINE_CURVE_WITH_KNOTS('',3,(#27901,#27902,#27903,#27904,#27905,
#27906,#27907,#27908,#27909,#27910,#27911,#27912,#27913,#27914,#27915,#27916,
#27917,#27918,#27919,#27920,#27921,#27922,#27923,#27924,#27925),
 .UNSPECIFIED.,.F.,.F.,(4,3,3,3,3,3,3,3,4),(120.49782124478,120.772613091602,
121.770733860954,122.768854630306,123.766975399658,124.76509616901,125.763216938362,
126.761337707714,126.78100655196),.UNSPECIFIED.);
#1088=B_SPLINE_CURVE_WITH_KNOTS('',3,(#27930,#27931,#27932,#27933,#27934,
#27935,#27936,#27937,#27938,#27939,#27940,#27941,#27942,#27943,#27944,#27945,
#27946,#27947,#27948,#27949,#27950,#27951),.UNSPECIFIED.,.F.,.F.,(4,3,3,
3,3,3,3,4),(-136.039821870902,-135.744424631883,-134.746303862531,-133.748183093179,
-132.750062323826,-131.751941554474,-130.753820785122,-129.756636563722),
 .UNSPECIFIED.);
#1089=B_SPLINE_CURVE_WITH_KNOTS('',3,(#27952,#27953,#27954,#27955,#27956,
#27957,#27958,#27959,#27960,#27961,#27962,#27963,#27964,#27965,#27966,#27967,
#27968,#27969,#27970,#27971,#27972,#27973),.UNSPECIFIED.,.F.,.F.,(4,3,3,
3,3,3,3,4),(126.78100655196,127.759458477066,128.757579246418,129.75570001577,
130.753820785122,131.751941554474,132.750062323826,133.06419185914),
 .UNSPECIFIED.);
#1090=B_SPLINE_CURVE_WITH_KNOTS('',3,(#27978,#27979,#27980,#27981,#27982,
#27983,#27984,#27985,#27986,#27987,#27988,#27989,#27990,#27991,#27992,#27993,
#27994,#27995,#27996,#27997,#27998,#27999),.UNSPECIFIED.,.F.,.F.,(4,3,3,
3,3,3,3,4),(-142.323007178082,-141.733149247995,-140.735028478643,-139.736907709291,
-138.738786939939,-137.740666170587,-136.742545401235,-136.039821870902),
 .UNSPECIFIED.);
#1091=B_SPLINE_CURVE_WITH_KNOTS('',3,(#28000,#28001,#28002,#28003,#28004,
#28005,#28006,#28007,#28008,#28009,#28010,#28011,#28012,#28013,#28014,#28015,
#28016,#28017,#28018,#28019,#28020,#28021),.UNSPECIFIED.,.F.,.F.,(4,3,3,
3,3,3,3,4),(133.06419185914,133.748183093179,134.746303862531,135.744424631883,
136.742545401235,137.740666170587,138.738786939939,139.347377166319),
 .UNSPECIFIED.);
#1092=B_SPLINE_CURVE_WITH_KNOTS('',3,(#28026,#28027,#28028,#28029,#28030,
#28031,#28032,#28033,#28034,#28035,#28036,#28037,#28038,#28039,#28040,#28041,
#28042,#28043,#28044,#28045,#28046,#28047),.UNSPECIFIED.,.F.,.F.,(4,3,3,
3,3,3,3,4),(-148.606192485261,-147.721873864108,-146.723753094756,-145.725632325403,
-144.727511556051,-143.729390786699,-142.731270017347,-142.323007178082),
 .UNSPECIFIED.);
#1093=B_SPLINE_CURVE_WITH_KNOTS('',3,(#28048,#28049,#28050,#28051,#28052,
#28053,#28054,#28055,#28056,#28057,#28058,#28059,#28060,#28061,#28062,#28063,
#28064,#28065,#28066,#28067,#28068,#28069),.UNSPECIFIED.,.F.,.F.,(4,3,3,
3,3,3,3,4),(139.347377166319,139.736907709291,140.735028478643,141.733149247995,
142.731270017347,143.729390786699,144.727511556051,145.630562473499),
 .UNSPECIFIED.);
#1094=B_SPLINE_CURVE_WITH_KNOTS('',3,(#28075,#28076,#28077,#28078),
 .UNSPECIFIED.,.F.,.F.,(4,4),(160.221225333079,160.262630845073),
 .UNSPECIFIED.);
#1095=B_SPLINE_CURVE_WITH_KNOTS('',3,(#28084,#28085,#28086,#28087,#28088,
#28089,#28090,#28091,#28092,#28093),.UNSPECIFIED.,.F.,.F.,(4,1,1,1,1,1,
1,4),(153.9380400259,154.346302865166,155.344423634518,156.34254440387,
157.340665173222,158.338785942574,159.336906711926,160.221225333079),
 .UNSPECIFIED.);
#1096=B_SPLINE_CURVE_WITH_KNOTS('',3,(#28096,#28097,#28098,#28099,#28100,
#28101,#28102,#28103,#28104),.UNSPECIFIED.,.F.,.F.,(4,1,1,1,1,1,4),(153.9380400259,
154.033109877805,155.031230647157,156.029351416509,157.027472185861,158.025592955213,
159.023713724565),.UNSPECIFIED.);
#1097=B_SPLINE_CURVE_WITH_KNOTS('',3,(#28109,#28110,#28111,#28112,#28113,
#28114,#28115,#28116,#28117,#28118),.UNSPECIFIED.,.F.,.F.,(4,1,1,1,1,1,
1,4),(147.65485471872,148.357578249053,149.355699018405,150.353819787757,
151.351940557109,152.350061326461,153.348182095814,153.9380400259),
 .UNSPECIFIED.);
#1098=B_SPLINE_CURVE_WITH_KNOTS('',3,(#28119,#28120,#28121,#28122,#28123,
#28124,#28125,#28126,#28127,#28128),.UNSPECIFIED.,.F.,.F.,(4,1,1,1,1,1,
1,4),(147.65485471872,148.044385261692,149.042506031044,150.040626800396,
151.038747569748,152.0368683391,153.034989108453,153.9380400259),
 .UNSPECIFIED.);
#1099=B_SPLINE_CURVE_WITH_KNOTS('',3,(#28133,#28134,#28135,#28136,#28137,
#28138,#28139,#28140,#28141,#28142),.UNSPECIFIED.,.F.,.F.,(4,1,1,1,1,1,
1,4),(141.371669411541,142.368853632941,143.366974402293,144.365095171645,
145.363215940997,146.361336710349,147.359457479701,147.65485471872),
 .UNSPECIFIED.);
#1100=B_SPLINE_CURVE_WITH_KNOTS('',3,(#28143,#28144,#28145,#28146,#28147,
#28148,#28149,#28150,#28151,#28152),.UNSPECIFIED.,.F.,.F.,(4,1,1,1,1,1,
1,4),(141.371669411541,142.05566064558,143.053781414932,144.051902184284,
145.050022953636,146.048143722988,147.04626449234,147.65485471872),
 .UNSPECIFIED.);
#1101=B_SPLINE_CURVE_WITH_KNOTS('',3,(#28157,#28158,#28159,#28160,#28161,
#28162,#28163,#28164,#28165,#28166,#28167),.UNSPECIFIED.,.F.,.F.,(4,1,1,
1,1,1,1,1,4),(135.088484104361,135.382008247476,136.380129016828,137.37824978618,
138.376370555532,139.374491324884,140.372612094236,141.370732863589,141.371669411541),
 .UNSPECIFIED.);
#1102=B_SPLINE_CURVE_WITH_KNOTS('',3,(#28168,#28169,#28170,#28171,#28172,
#28173,#28174,#28175,#28176,#28177),.UNSPECIFIED.,.F.,.F.,(4,1,1,1,1,1,
1,4),(135.088484104361,136.066936029467,137.065056798819,138.063177568171,
139.061298337523,140.059419106876,141.057539876228,141.371669411541),
 .UNSPECIFIED.);
#1103=B_SPLINE_CURVE_WITH_KNOTS('',3,(#28182,#28183,#28184,#28185,#28186,
#28187,#28188,#28189,#28190,#28191),.UNSPECIFIED.,.F.,.F.,(4,1,1,1,1,1,
1,4),(128.805298797182,129.393283631364,130.391404400716,131.389525170068,
132.38764593942,133.385766708772,134.383887478124,135.088484104361),
 .UNSPECIFIED.);
#1104=B_SPLINE_CURVE_WITH_KNOTS('',3,(#28192,#28193,#28194,#28195,#28196,
#28197,#28198,#28199,#28200,#28201,#28202),.UNSPECIFIED.,.F.,.F.,(4,1,1,
1,1,1,1,1,4),(128.805298797182,129.080090644003,130.078211413355,131.076332182707,
132.074452952059,133.072573721411,134.070694490763,135.068815260115,135.088484104361),
 .UNSPECIFIED.);
#1105=B_SPLINE_CURVE_WITH_KNOTS('',3,(#28207,#28208,#28209,#28210,#28211,
#28212,#28213,#28214,#28215,#28216),.UNSPECIFIED.,.F.,.F.,(4,1,1,1,1,1,
1,4),(122.522113490002,123.404559015251,124.402679784603,125.400800553955,
126.398921323307,127.397042092659,128.395162862012,128.805298797182),
 .UNSPECIFIED.);
#1106=B_SPLINE_CURVE_WITH_KNOTS('',3,(#28217,#28218,#28219,#28220,#28221,
#28222,#28223,#28224,#28225,#28226),.UNSPECIFIED.,.F.,.F.,(4,1,1,1,1,1,
1,4),(122.522113490002,123.09136602789,124.089486797242,125.087607566594,
126.085728335946,127.083849105298,128.081969874651,128.805298797182),
 .UNSPECIFIED.);
#1107=B_SPLINE_CURVE_WITH_KNOTS('',3,(#28231,#28232,#28233,#28234,#28235,
#28236,#28237,#28238,#28239,#28240,#28241),.UNSPECIFIED.,.F.,.F.,(4,1,1,
1,1,1,1,1,4),(116.238928182822,116.417713629787,117.415834399139,118.413955168491,
119.412075937843,120.410196707195,121.408317476547,122.406438245899,122.522113490002),
 .UNSPECIFIED.);
#1108=B_SPLINE_CURVE_WITH_KNOTS('',3,(#28242,#28243,#28244,#28245,#28246,
#28247,#28248,#28249,#28250,#28251),.UNSPECIFIED.,.F.,.F.,(4,1,1,1,1,1,
1,4),(116.238928182822,117.102641411778,118.10076218113,119.098882950482,
120.097003719834,121.095124489186,122.093245258538,122.522113490002),
 .UNSPECIFIED.);
#1109=B_SPLINE_CURVE_WITH_KNOTS('',3,(#28256,#28257,#28258,#28259,#28260,
#28261,#28262,#28263,#28264,#28265),.UNSPECIFIED.,.F.,.F.,(4,1,1,1,1,1,
1,4),(109.955742875643,110.428989013674,111.427109783026,112.425230552378,
113.42335132173,114.421472091082,115.419592860435,116.238928182822),
 .UNSPECIFIED.);
#1110=B_SPLINE_CURVE_WITH_KNOTS('',3,(#28266,#28267,#28268,#28269,#28270,
#28271,#28272,#28273,#28274,#28275,#28276),.UNSPECIFIED.,.F.,.F.,(4,1,1,
1,1,1,1,1,4),(109.955742875643,110.115796026313,111.113916795665,112.112037565017,
113.110158334369,114.108279103721,115.106399873074,116.104520642426,116.238928182822),
 .UNSPECIFIED.);
#1111=B_SPLINE_CURVE_WITH_KNOTS('',3,(#28281,#28282,#28283,#28284,#28285,
#28286,#28287,#28288,#28289,#28290),.UNSPECIFIED.,.F.,.F.,(4,1,1,1,1,1,
1,4),(103.672557568463,104.440264397562,105.438385166914,106.436505936266,
107.434626705618,108.43274747497,109.430868244322,109.955742875643),
 .UNSPECIFIED.);
#1112=B_SPLINE_CURVE_WITH_KNOTS('',3,(#28291,#28292,#28293,#28294,#28295,
#28296,#28297,#28298,#28299,#28300),.UNSPECIFIED.,.F.,.F.,(4,1,1,1,1,1,
1,4),(103.672557568463,104.127071410201,105.125192179553,106.123312948905,
107.121433718257,108.119554487609,109.117675256961,109.955742875643),
 .UNSPECIFIED.);
#1113=B_SPLINE_CURVE_WITH_KNOTS('',3,(#28305,#28306,#28307,#28308,#28309,
#28310,#28311,#28312,#28313,#28314,#28315),.UNSPECIFIED.,.F.,.F.,(4,1,1,
1,1,1,1,1,4),(97.3893722612836,97.4534190120971,98.4515397814492,99.4496605508013,
100.447781320153,101.445902089505,102.444022858857,103.44214362821,103.672557568463),
 .UNSPECIFIED.);
#1114=B_SPLINE_CURVE_WITH_KNOTS('',3,(#28316,#28317,#28318,#28319,#28320,
#28321,#28322,#28323,#28324,#28325),.UNSPECIFIED.,.F.,.F.,(4,1,1,1,1,1,
1,4),(97.3893722612836,98.1383467940882,99.1364675634403,100.134588332792,
101.132709102144,102.130829871497,103.128950640849,103.672557568463),
 .UNSPECIFIED.);
#1115=B_SPLINE_CURVE_WITH_KNOTS('',3,(#28330,#28331,#28332,#28333,#28334,
#28335,#28336,#28337,#28338,#28339),.UNSPECIFIED.,.F.,.F.,(4,1,1,1,1,1,
1,4),(91.106186954104,91.4646943959846,92.4628151653367,93.4609359346888,
94.4590567040409,95.4571774733929,96.455298242745,97.3893722612836),
 .UNSPECIFIED.);
#1116=B_SPLINE_CURVE_WITH_KNOTS('',3,(#28340,#28341,#28342,#28343,#28344,
#28345,#28346,#28347,#28348,#28349,#28350),.UNSPECIFIED.,.F.,.F.,(4,1,1,
1,1,1,1,1,4),(91.106186954104,91.1515014086236,92.1496221779757,93.1477429473278,
94.1458637166799,95.143984486032,96.142105255384,97.1402260247361,97.3893722612836),
 .UNSPECIFIED.);
#1117=B_SPLINE_CURVE_WITH_KNOTS('',3,(#28355,#28356,#28357,#28358,#28359,
#28360,#28361,#28362,#28363,#28364),.UNSPECIFIED.,.F.,.F.,(4,1,1,1,1,1,
1,4),(84.8230016469245,85.4759697798722,86.4740905492242,87.4722113185763,
88.4703320879284,89.4684528572805,90.4665736266326,91.106186954104),
 .UNSPECIFIED.);
#1118=B_SPLINE_CURVE_WITH_KNOTS('',3,(#28365,#28366,#28367,#28368,#28369,
#28370,#28371,#28372,#28373,#28374),.UNSPECIFIED.,.F.,.F.,(4,1,1,1,1,1,
1,4),(84.8230016469245,85.1627767925112,86.1608975618633,87.1590183312153,
88.1571391005674,89.1552598699195,90.1533806392716,91.106186954104),
 .UNSPECIFIED.);
#1119=B_SPLINE_CURVE_WITH_KNOTS('',3,(#28379,#28380,#28381,#28382,#28383,
#28384,#28385,#28386,#28387,#28388),.UNSPECIFIED.,.F.,.F.,(4,1,1,1,1,1,
1,4),(78.5398163397449,79.4872451637597,80.4853659331118,81.4834867024638,
82.4816074718159,83.479728241168,84.4778490105201,84.8230016469245),
 .UNSPECIFIED.);
#1120=B_SPLINE_CURVE_WITH_KNOTS('',3,(#28389,#28390,#28391,#28392,#28393,
#28394,#28395,#28396,#28397,#28398),.UNSPECIFIED.,.F.,.F.,(4,1,1,1,1,1,
1,4),(78.5398163397449,79.1740521763987,80.1721729457508,81.1702937151029,
82.1684144844549,83.166535253807,84.1646560231591,84.8230016469245),
 .UNSPECIFIED.);
#1121=B_SPLINE_CURVE_WITH_KNOTS('',3,(#28403,#28404,#28405,#28406,#28407,
#28408,#28409,#28410,#28411,#28412,#28413),.UNSPECIFIED.,.F.,.F.,(4,1,1,
1,1,1,1,1,4),(72.2566310325653,72.5003997782951,73.4985205476472,74.4966413169993,
75.4947620863514,76.4928828557034,77.4910036250555,78.4891243944076,78.5398163397449),
 .UNSPECIFIED.);
#1122=B_SPLINE_CURVE_WITH_KNOTS('',3,(#28414,#28415,#28416,#28417,#28418,
#28419,#28420,#28421,#28422,#28423),.UNSPECIFIED.,.F.,.F.,(4,1,1,1,1,1,
1,4),(72.2566310325653,73.1853275602862,74.1834483296383,75.1815690989904,
76.1796898683425,77.1778106376945,78.1759314070466,78.5398163397449),
 .UNSPECIFIED.);
#1123=B_SPLINE_CURVE_WITH_KNOTS('',3,(#28428,#28429,#28430,#28431,#28432,
#28433,#28434,#28435,#28436,#28437),.UNSPECIFIED.,.F.,.F.,(4,1,1,1,1,1,
1,4),(65.9734457253857,66.5116751621827,67.5097959315347,68.5079167008868,
69.5060374702389,70.504158239591,71.502279008943,72.2566310325653),
 .UNSPECIFIED.);
#1124=B_SPLINE_CURVE_WITH_KNOTS('',3,(#28438,#28439,#28440,#28441,#28442,
#28443,#28444,#28445,#28446,#28447,#28448),.UNSPECIFIED.,.F.,.F.,(4,1,1,
1,1,1,1,1,4),(65.9734457253857,66.1984821748217,67.1966029441738,68.1947237135258,
69.1928444828779,70.19096525223,71.1890860215821,72.1872067909342,72.2566310325653),
 .UNSPECIFIED.);
#1125=B_SPLINE_CURVE_WITH_KNOTS('',3,(#28453,#28454,#28455,#28456,#28457,
#28458,#28459,#28460,#28461,#28462),.UNSPECIFIED.,.F.,.F.,(4,1,1,1,1,1,
1,4),(59.6902604182061,60.5229505460702,61.5210713154223,62.5191920847743,
63.5173128541264,64.5154336234785,65.5135543928306,65.9734457253857),
 .UNSPECIFIED.);
#1126=B_SPLINE_CURVE_WITH_KNOTS('',3,(#28463,#28464,#28465,#28466,#28467,
#28468,#28469,#28470,#28471,#28472),.UNSPECIFIED.,.F.,.F.,(4,1,1,1,1,1,
1,4),(59.6902604182061,60.2097575587092,61.2078783280613,62.2059990974134,
63.2041198667654,64.2022406361175,65.2003614054696,65.9734457253857),
 .UNSPECIFIED.);
#1127=B_SPLINE_CURVE_WITH_KNOTS('',3,(#28477,#28478,#28479,#28480,#28481,
#28482,#28483,#28484,#28485,#28486,#28487),.UNSPECIFIED.,.F.,.F.,(4,1,1,
1,1,1,1,1,4),(53.4070751110265,53.5361051606056,54.5342259299577,55.5323466993098,
56.5304674686619,57.528588238014,58.526709007366,59.5248297767181,59.6902604182061),
 .UNSPECIFIED.);
#1128=B_SPLINE_CURVE_WITH_KNOTS('',3,(#28488,#28489,#28490,#28491,#28492,
#28493,#28494,#28495,#28496,#28497),.UNSPECIFIED.,.F.,.F.,(4,1,1,1,1,1,
1,4),(53.4070751110265,54.2210329425967,55.2191537119488,56.2172744813009,
57.215395250653,58.213516020005,59.2116367893571,59.6902604182061),
 .UNSPECIFIED.);
#1129=B_SPLINE_CURVE_WITH_KNOTS('',3,(#28502,#28503,#28504,#28505,#28506,
#28507,#28508,#28509,#28510,#28511),.UNSPECIFIED.,.F.,.F.,(4,1,1,1,1,1,
1,4),(47.1238898038469,47.5473805444932,48.5455013138453,49.5436220831973,
50.5417428525494,51.5398636219015,52.5379843912536,53.4070751110265),
 .UNSPECIFIED.);
#1130=B_SPLINE_CURVE_WITH_KNOTS('',3,(#28512,#28513,#28514,#28515,#28516,
#28517,#28518,#28519,#28520,#28521,#28522),.UNSPECIFIED.,.F.,.F.,(4,1,1,
1,1,1,1,1,4),(47.1238898038469,47.2341875571322,48.2323083264843,49.2304290958363,
50.2285498651884,51.2266706345405,52.2247914038926,53.2229121732447,53.4070751110265),
 .UNSPECIFIED.);
#1131=B_SPLINE_CURVE_WITH_KNOTS('',3,(#28527,#28528,#28529,#28530,#28531,
#28532,#28533,#28534,#28535,#28536),.UNSPECIFIED.,.F.,.F.,(4,1,1,1,1,1,
1,4),(40.8407044966673,41.5586559283807,42.5567766977328,43.5548974670848,
44.5530182364369,45.551139005789,46.5492597751411,47.1238898038469),
 .UNSPECIFIED.);
#1132=B_SPLINE_CURVE_WITH_KNOTS('',3,(#28537,#28538,#28539,#28540,#28541,
#28542,#28543,#28544,#28545,#28546),.UNSPECIFIED.,.F.,.F.,(4,1,1,1,1,1,
1,4),(40.8407044966673,41.2454629410197,42.2435837103718,43.2417044797239,
44.2398252490759,45.237946018428,46.2360667877801,47.1238898038469),
 .UNSPECIFIED.);
#1133=B_SPLINE_CURVE_WITH_KNOTS('',3,(#28551,#28552,#28553,#28554,#28555,
#28556,#28557,#28558,#28559,#28560,#28561),.UNSPECIFIED.,.F.,.F.,(4,1,1,
1,1,1,1,1,4),(34.5575191894877,34.5718105429161,35.5699313122682,36.5680520816203,
37.5661728509724,38.5642936203245,39.5624143896765,40.5605351590286,40.8407044966673),
 .UNSPECIFIED.);
#1134=B_SPLINE_CURVE_WITH_KNOTS('',3,(#28562,#28563,#28564,#28565,#28566,
#28567,#28568,#28569,#28570,#28571),.UNSPECIFIED.,.F.,.F.,(4,1,1,1,1,1,
1,4),(34.5575191894877,35.2567383249072,36.2548590942593,37.2529798636114,
38.2511006329635,39.2492214023156,40.2473421716676,40.8407044966673),
 .UNSPECIFIED.);
#1135=B_SPLINE_CURVE_WITH_KNOTS('',3,(#28576,#28577,#28578,#28579,#28580,
#28581,#28582,#28583,#28584,#28585),.UNSPECIFIED.,.F.,.F.,(4,1,1,1,1,1,
1,4),(28.2743338823081,28.5830859268037,29.5812066961557,30.5793274655078,
31.5774482348599,32.575569004212,33.5736897735641,34.5575191894877),
 .UNSPECIFIED.);
#1136=B_SPLINE_CURVE_WITH_KNOTS('',3,(#28586,#28587,#28588,#28589,#28590,
#28591,#28592,#28593,#28594,#28595),.UNSPECIFIED.,.F.,.F.,(4,1,1,1,1,1,
1,4),(28.2743338823081,29.2680137087948,30.2661344781468,31.2642552474989,
32.262376016851,33.2604967862031,34.2586175555552,34.5575191894877),
 .UNSPECIFIED.);
#1137=B_SPLINE_CURVE_WITH_KNOTS('',3,(#28600,#28601,#28602,#28603,#28604,
#28605,#28606,#28607,#28608,#28609),.UNSPECIFIED.,.F.,.F.,(4,1,1,1,1,1,
1,4),(21.9911485751285,22.5943613106912,23.5924820800433,24.5906028493954,
25.5887236187474,26.5868443880995,27.5849651574516,28.2743338823081),
 .UNSPECIFIED.);
#1138=B_SPLINE_CURVE_WITH_KNOTS('',3,(#28610,#28611,#28612,#28613,#28614,
#28615,#28616,#28617,#28618,#28619,#28620),.UNSPECIFIED.,.F.,.F.,(4,1,1,
1,1,1,1,1,4),(21.9911485751285,22.2811683233302,23.2792890926823,24.2774098620344,
25.2755306313865,26.2736514007385,27.2717721700906,28.2698929394427,28.2743338823081),
 .UNSPECIFIED.);
#1139=B_SPLINE_CURVE_WITH_KNOTS('',3,(#28625,#28626,#28627,#28628,#28629,
#28630,#28631,#28632,#28633,#28634),.UNSPECIFIED.,.F.,.F.,(4,1,1,1,1,1,
1,4),(15.707963267949,16.6056366945787,17.6037574639308,18.6018782332829,
19.599999002635,20.598119771987,21.5962405413391,21.9911485751285),
 .UNSPECIFIED.);
#1140=B_SPLINE_CURVE_WITH_KNOTS('',3,(#28635,#28636,#28637,#28638,#28639,
#28640,#28641,#28642,#28643,#28644),.UNSPECIFIED.,.F.,.F.,(4,1,1,1,1,1,
1,4),(15.707963267949,16.2924437072177,17.2905644765698,18.2886852459219,
19.286806015274,20.2849267846261,21.2830475539781,21.9911485751285),
 .UNSPECIFIED.);
#1141=B_SPLINE_CURVE_WITH_KNOTS('',3,(#29262,#29263,#29264,#29265,#29266,
#29267,#29268,#29269,#29270,#29271,#29272,#29273,#29274,#29275,#29276,#29277,
#29278,#29279,#29280,#29281,#29282,#29283,#29284,#29285,#29286,#29287,#29288,
#29289,#29290,#29291,#29292,#29293,#29294,#29295,#29296,#29297,#29298,#29299,
#29300,#29301,#29302,#29303,#29304,#29305,#29306,#29307,#29308,#29309,#29310,
#29311,#29312,#29313,#29314,#29315,#29316,#29317,#29318,#29319),
 .UNSPECIFIED.,.F.,.F.,(4,3,3,3,3,3,3,3,3,3,3,3,3,3,3,3,3,3,3,4),(-0.552745378375043,
-0.531489243744843,-0.495108433985232,-0.477867666908701,-0.459926783852948,
-0.40834015484357,-0.390564261242345,-0.340650422189222,-0.308207347384289,
-0.294851172015872,-0.28154967607649,-0.252476072145833,-0.202914686431521,
-0.190042837184204,-0.142532127888153,-0.10590131786763,-0.092666137023641,
-0.0463330685118205,-0.0028441867201021,0.),.UNSPECIFIED.);
#1142=B_SPLINE_CURVE_WITH_KNOTS('',3,(#29320,#29321,#29322,#29323,#29324,
#29325,#29326,#29327,#29328,#29329,#29330,#29331,#29332),.UNSPECIFIED.,
 .F.,.F.,(4,3,3,3,4),(145.630562473499,145.725632325403,146.723753094756,
147.721873864108,148.647597997255),.UNSPECIFIED.);
#1143=B_SPLINE_CURVE_WITH_KNOTS('',3,(#29334,#29335,#29336,#29337,#29338,
#29339,#29340,#29341,#29342,#29343,#29344,#29345,#29346,#29347,#29348,#29349,
#29350,#29351,#29352,#29353,#29354,#29355,#29356,#29357,#29358,#29359,#29360,
#29361,#29362,#29363,#29364,#29365,#29366,#29367,#29368,#29369,#29370,#29371,
#29372,#29373,#29374,#29375,#29376,#29377,#29378,#29379,#29380,#29381,#29382,
#29383,#29384,#29385,#29386,#29387,#29388),.UNSPECIFIED.,.F.,.F.,(4,3,3,
3,3,3,3,3,3,3,3,3,3,3,3,3,3,3,4),(-0.555272788399391,-0.537829475145404,
-0.501151444327474,-0.480433685752521,-0.449607979278525,-0.430089933902533,
-0.415584630121194,-0.367513977288793,-0.334452546673387,-0.315854971100898,
-0.282472195537201,-0.247163171095051,-0.224831098912879,-0.211454760083625,
-0.161528020768348,-0.11601494941692,-0.102547348706884,-0.050144009897631,
0.),.UNSPECIFIED.);
#1144=B_SPLINE_CURVE_WITH_KNOTS('',3,(#29389,#29390,#29391,#29392,#29393,
#29394,#29395,#29396,#29397),.UNSPECIFIED.,.F.,.F.,(4,1,1,1,1,1,4),(10.3761157273103,
11.3018398604573,12.2999606298094,13.2980813991615,14.2962021685136,15.2943229378657,
15.707963267949),.UNSPECIFIED.);
#1145=B_SPLINE_CURVE_WITH_KNOTS('',3,(#29403,#29404,#29405,#29406,#29407,
#29408,#29409,#29410,#29411,#29412,#29413,#29414,#29415,#29416,#29417,#29418,
#29419,#29420,#29421,#29422,#29423,#29424,#29425,#29426,#29427,#29428,#29429,
#29430,#29431,#29432,#29433,#29434,#29435,#29436,#29437,#29438,#29439,#29440,
#29441,#29442,#29443,#29444,#29445,#29446,#29447,#29448,#29449,#29450,#29451,
#29452,#29453,#29454,#29455,#29456,#29457,#29458,#29459,#29460),
 .UNSPECIFIED.,.F.,.F.,(4,3,3,3,3,3,3,3,3,3,3,3,3,3,3,3,3,3,3,4),(-0.552745378375056,
-0.531489243744835,-0.495108428311827,-0.477867651520537,-0.45992677828748,
-0.408340146860344,-0.39056425606813,-0.34065040901948,-0.308207314423746,
-0.294851132888488,-0.28154966653563,-0.252476072145832,-0.202914855082696,
-0.190043155762275,-0.142532366821707,-0.105901640544872,-0.0926664448836297,
-0.0463332224418149,-0.00284436592965125,0.),.UNSPECIFIED.);
#1146=B_SPLINE_CURVE_WITH_KNOTS('',3,(#29463,#29464,#29465,#29466,#29467,
#29468,#29469,#29470),.UNSPECIFIED.,.F.,.F.,(4,1,1,1,1,4),(11.6150328478183,
12.6131536171704,13.6112743865225,14.6093951558746,15.6075159252266,15.707963267949),
 .UNSPECIFIED.);
#1147=B_SPLINE_CURVE_WITH_KNOTS('',3,(#30088,#30089,#30090,#30091,#30092,
#30093,#30094,#30095,#30096,#30097,#30098,#30099,#30100,#30101,#30102,#30103,
#30104,#30105,#30106,#30107,#30108,#30109,#30110,#30111,#30112,#30113,#30114,
#30115,#30116,#30117,#30118,#30119,#30120,#30121,#30122,#30123,#30124,#30125,
#30126,#30127,#30128,#30129,#30130,#30131,#30132,#30133,#30134,#30135,#30136,
#30137,#30138,#30139,#30140,#30141,#30142),.UNSPECIFIED.,.F.,.F.,(4,3,3,
3,3,3,3,3,3,3,3,3,3,3,3,3,3,3,4),(-0.55527278839943,-0.537829475145452,
-0.501151443157722,-0.480433683572202,-0.449608208717037,-0.430090720039549,
-0.415584982436066,-0.367514333548957,-0.334452908269952,-0.315854921314816,
-0.282472195537241,-0.247163171095086,-0.224831104408066,-0.211454765807094,
-0.161528018350323,-0.116014945472013,-0.102547346883912,-0.0501440159489521,
0.),.UNSPECIFIED.);
#1148=B_SPLINE_CURVE_WITH_KNOTS('',3,(#30143,#30144,#30145,#30146,#30147,
#30148,#30149,#30150,#30151,#30152),.UNSPECIFIED.,.F.,.F.,(4,3,3,4),(-150.716236172164,
-149.718115402812,-148.71999463346,-148.606192485261),.UNSPECIFIED.);
#1149=B_SPLINE_CURVE_WITH_KNOTS('',3,(#30994,#30995,#30996,#30997,#30998,
#30999),.UNSPECIFIED.,.F.,.F.,(4,2,4),(-0.0356445426705879,-0.017820065955887,
0.),.UNSPECIFIED.);
#1150=B_SPLINE_CURVE_WITH_KNOTS('',3,(#31000,#31001,#31002,#31003,#31004,
#31005),.UNSPECIFIED.,.F.,.F.,(4,2,4),(-0.0356445406593133,-0.0178242377363697,
0.),.UNSPECIFIED.);
#1151=B_SPLINE_CURVE_WITH_KNOTS('',3,(#31009,#31010,#31011,#31012,#31013,
#31014),.UNSPECIFIED.,.F.,.F.,(4,2,4),(-0.0356445426646998,-0.0178200659542505,
0.),.UNSPECIFIED.);
#1152=B_SPLINE_CURVE_WITH_KNOTS('',3,(#31016,#31017,#31018,#31019,#31020,
#31021),.UNSPECIFIED.,.F.,.F.,(4,2,4),(-0.0356445406608173,-0.0178242377372387,
0.),.UNSPECIFIED.);
#1153=B_SPLINE_CURVE_WITH_KNOTS('',3,(#31028,#31029,#31030,#31031,#31032,
#31033),.UNSPECIFIED.,.F.,.F.,(4,2,4),(-0.035644542668606,-0.0178200659552084,
0.),.UNSPECIFIED.);
#1154=B_SPLINE_CURVE_WITH_KNOTS('',3,(#31034,#31035,#31036,#31037,#31038,
#31039),.UNSPECIFIED.,.F.,.F.,(4,2,4),(-0.0356445406611976,-0.0178242377369016,
0.),.UNSPECIFIED.);
#1155=B_SPLINE_CURVE_WITH_KNOTS('',3,(#31043,#31044,#31045,#31046,#31047,
#31048),.UNSPECIFIED.,.F.,.F.,(4,2,4),(-0.0356445426695261,-0.0178200659558121,
0.),.UNSPECIFIED.);
#1156=B_SPLINE_CURVE_WITH_KNOTS('',3,(#31050,#31051,#31052,#31053,#31054,
#31055),.UNSPECIFIED.,.F.,.F.,(4,2,4),(-0.0356445406606661,-0.0178242377367645,
0.),.UNSPECIFIED.);
#1157=B_SPLINE_CURVE_WITH_KNOTS('',3,(#31062,#31063,#31064,#31065,#31066,
#31067),.UNSPECIFIED.,.F.,.F.,(4,2,4),(-0.0356445426677898,-0.0178200659551202,
0.),.UNSPECIFIED.);
#1158=B_SPLINE_CURVE_WITH_KNOTS('',3,(#31068,#31069,#31070,#31071,#31072,
#31073),.UNSPECIFIED.,.F.,.F.,(4,2,4),(-0.0356445406615696,-0.0178242377363734,
0.),.UNSPECIFIED.);
#1159=B_SPLINE_CURVE_WITH_KNOTS('',3,(#31077,#31078,#31079,#31080,#31081,
#31082),.UNSPECIFIED.,.F.,.F.,(4,2,4),(-0.0356445426680788,-0.017820065955108,
0.),.UNSPECIFIED.);
#1160=B_SPLINE_CURVE_WITH_KNOTS('',3,(#31084,#31085,#31086,#31087,#31088,
#31089),.UNSPECIFIED.,.F.,.F.,(4,2,4),(-0.0356445406623922,-0.0178242377374904,
0.),.UNSPECIFIED.);
#1161=B_SPLINE_CURVE_WITH_KNOTS('',3,(#31113,#31114,#31115,#31116,#31117,
#31118,#31119,#31120,#31121,#31122,#31123,#31124,#31125,#31126,#31127,#31128,
#31129,#31130,#31131,#31132,#31133,#31134,#31135,#31136,#31137),
 .UNSPECIFIED.,.F.,.F.,(4,3,3,3,3,3,3,3,4),(1.38777878078145E-17,0.0499520104369165,
0.0579096339663456,0.0689507685252385,0.0901012807338169,0.116325803406286,
0.146260951142593,0.196900647008064,0.212043967873001),.UNSPECIFIED.);
#1162=B_SPLINE_CURVE_WITH_KNOTS('',3,(#31138,#31139,#31140,#31141),
 .UNSPECIFIED.,.F.,.F.,(4,4),(0.50492078692473,0.681229914591334),
 .UNSPECIFIED.);
#1163=B_SPLINE_CURVE_WITH_KNOTS('',3,(#31142,#31143,#31144,#31145,#31146),
 .UNSPECIFIED.,.F.,.F.,(4,1,4),(-0.679321786705464,-0.343792306535718,-0.0926222283799249),
 .UNSPECIFIED.);
#1164=B_SPLINE_CURVE_WITH_KNOTS('',3,(#31147,#31148,#31149,#31150),
 .UNSPECIFIED.,.F.,.F.,(4,4),(0.0907141004940068,0.26702322816061),
 .UNSPECIFIED.);
#1165=B_SPLINE_CURVE_WITH_KNOTS('',3,(#31181,#31182,#31183,#31184,#31185,
#31186,#31187,#31188,#31189,#31190,#31191,#31192,#31193,#31194,#31195,#31196,
#31197,#31198,#31199,#31200,#31201,#31202,#31203,#31204,#31205),
 .UNSPECIFIED.,.F.,.F.,(4,3,3,3,3,3,3,3,4),(0.,0.0499552658273372,0.0579096339663306,
0.0689507685252128,0.0901012807337863,0.116325803406243,0.146260951142533,
0.196900647007959,0.212043967872853),.UNSPECIFIED.);
#1166=B_SPLINE_CURVE_WITH_KNOTS('',3,(#31206,#31207,#31208,#31209),
 .UNSPECIFIED.,.F.,.F.,(4,4),(0.504920786924729,0.681229914591334),
 .UNSPECIFIED.);
#1167=B_SPLINE_CURVE_WITH_KNOTS('',3,(#31210,#31211,#31212,#31213,#31214),
 .UNSPECIFIED.,.F.,.F.,(4,1,4),(-0.679321786705464,-0.343792306535718,-0.092622228379925),
 .UNSPECIFIED.);
#1168=B_SPLINE_CURVE_WITH_KNOTS('',3,(#31215,#31216,#31217,#31218),
 .UNSPECIFIED.,.F.,.F.,(4,4),(0.0907141004940068,0.26702322816061),
 .UNSPECIFIED.);
#1169=B_SPLINE_CURVE_WITH_KNOTS('',3,(#31241,#31242,#31243,#31244,#31245,
#31246,#31247,#31248,#31249,#31250,#31251,#31252,#31253,#31254,#31255,#31256,
#31257,#31258,#31259,#31260,#31261,#31262,#31263,#31264,#31265),
 .UNSPECIFIED.,.F.,.F.,(4,3,3,3,3,3,3,3,4),(0.,0.0499520104360042,0.0579096339663052,
0.0689507685251914,0.0901012807337567,0.116325803406213,0.14626095114252,
0.196900647008034,0.212043967872961),.UNSPECIFIED.);
#1170=B_SPLINE_CURVE_WITH_KNOTS('',3,(#31266,#31267,#31268,#31269),
 .UNSPECIFIED.,.F.,.F.,(4,4),(0.50492078692473,0.681229914591334),
 .UNSPECIFIED.);
#1171=B_SPLINE_CURVE_WITH_KNOTS('',3,(#31270,#31271,#31272,#31273,#31274),
 .UNSPECIFIED.,.F.,.F.,(4,1,4),(-0.679321786705465,-0.343792306535719,-0.092622228379925),
 .UNSPECIFIED.);
#1172=B_SPLINE_CURVE_WITH_KNOTS('',3,(#31275,#31276,#31277,#31278),
 .UNSPECIFIED.,.F.,.F.,(4,4),(0.0907141004940071,0.26702322816061),
 .UNSPECIFIED.);
#1173=B_SPLINE_CURVE_WITH_KNOTS('',3,(#31317,#31318,#31319,#31320,#31321,
#31322,#31323,#31324,#31325,#31326,#31327,#31328,#31329,#31330,#31331,#31332,
#31333,#31334,#31335,#31336,#31337,#31338,#31339,#31340,#31341),
 .UNSPECIFIED.,.F.,.F.,(4,3,3,3,3,3,3,3,4),(0.,0.0501067129681924,0.0579096339662997,
0.0901012807337445,0.116325803406229,0.14310556044029,0.146260951142586,
0.196900647008164,0.212043967873065),.UNSPECIFIED.);
#1174=B_SPLINE_CURVE_WITH_KNOTS('',3,(#31342,#31343,#31344,#31345),
 .UNSPECIFIED.,.F.,.F.,(4,4),(0.50492078692473,0.681229914591334),
 .UNSPECIFIED.);
#1175=B_SPLINE_CURVE_WITH_KNOTS('',3,(#31346,#31347,#31348,#31349,#31350),
 .UNSPECIFIED.,.F.,.F.,(4,1,4),(-0.679321786705464,-0.428151708549622,-0.0926222283799251),
 .UNSPECIFIED.);
#1176=B_SPLINE_CURVE_WITH_KNOTS('',3,(#31351,#31352,#31353,#31354),
 .UNSPECIFIED.,.F.,.F.,(4,4),(0.0907141004940069,0.267023228160609),
 .UNSPECIFIED.);
#1177=B_SPLINE_CURVE_WITH_KNOTS('',3,(#31377,#31378,#31379,#31380,#31381,
#31382,#31383,#31384,#31385,#31386,#31387,#31388,#31389),.UNSPECIFIED.,
 .F.,.F.,(4,3,3,3,4),(0.,0.050107747114841,0.0579096339663157,0.0901012807337753,
0.106028581745725),.UNSPECIFIED.);
#1178=B_SPLINE_CURVE_WITH_KNOTS('',3,(#31391,#31392,#31393,#31394,#31395,
#31396,#31397,#31398,#31399,#31400,#31401,#31402,#31403,#31404,#31405,#31406),
 .UNSPECIFIED.,.F.,.F.,(4,3,3,3,3,4),(0.106028581745725,0.11632580340628,
0.143105560440363,0.146260951142647,0.196900647008195,0.212043967873119),
 .UNSPECIFIED.);
#1179=B_SPLINE_CURVE_WITH_KNOTS('',3,(#31407,#31408,#31409,#31410),
 .UNSPECIFIED.,.F.,.F.,(4,4),(0.50492078692473,0.681229914591334),
 .UNSPECIFIED.);
#1180=B_SPLINE_CURVE_WITH_KNOTS('',3,(#31411,#31412,#31413,#31414,#31415),
 .UNSPECIFIED.,.F.,.F.,(4,1,4),(-0.679321786705464,-0.428151708549622,-0.0926222283799252),
 .UNSPECIFIED.);
#1181=B_SPLINE_CURVE_WITH_KNOTS('',3,(#31416,#31417,#31418,#31419),
 .UNSPECIFIED.,.F.,.F.,(4,4),(0.090714100494007,0.26702322816061),
 .UNSPECIFIED.);
#1182=B_SPLINE_CURVE_WITH_KNOTS('',3,(#31458,#31459,#31460,#31461,#31462,
#31463,#31464,#31465,#31466,#31467,#31468,#31469,#31470,#31471,#31472,#31473,
#31474,#31475,#31476,#31477,#31478,#31479,#31480,#31481,#31482),
 .UNSPECIFIED.,.F.,.F.,(4,3,3,3,3,3,3,3,4),(0.,0.0499520104361464,0.0579096339662874,
0.0689507685251644,0.0901012807337523,0.116325803406236,0.146260951142573,
0.196900647008118,0.21204396787299),.UNSPECIFIED.);
#1183=B_SPLINE_CURVE_WITH_KNOTS('',3,(#31483,#31484,#31485,#31486),
 .UNSPECIFIED.,.F.,.F.,(4,4),(0.504920786924729,0.681229914591334),
 .UNSPECIFIED.);
#1184=B_SPLINE_CURVE_WITH_KNOTS('',3,(#31487,#31488,#31489,#31490,#31491),
 .UNSPECIFIED.,.F.,.F.,(4,1,4),(-0.679321786705464,-0.343792306535719,-0.0926222283799251),
 .UNSPECIFIED.);
#1185=B_SPLINE_CURVE_WITH_KNOTS('',3,(#31492,#31493,#31494,#31495),
 .UNSPECIFIED.,.F.,.F.,(4,4),(0.0907141004940075,0.26702322816061),
 .UNSPECIFIED.);
#1186=B_SPLINE_SURFACE_WITH_KNOTS('',3,3,((#16683,#16684,#16685,#16686),
(#16687,#16688,#16689,#16690),(#16691,#16692,#16693,#16694),(#16695,#16696,
#16697,#16698)),.UNSPECIFIED.,.F.,.F.,.F.,(4,4),(4,4),(0.,1.),(-5.39792313687514,
-5.36678788880707),.UNSPECIFIED.);
#1187=B_SPLINE_SURFACE_WITH_KNOTS('',3,3,((#16713,#16714,#16715,#16716),
(#16717,#16718,#16719,#16720),(#16721,#16722,#16723,#16724),(#16725,#16726,
#16727,#16728)),.UNSPECIFIED.,.F.,.F.,.F.,(4,4),(4,4),(0.,1.),(0.,1.),
 .UNSPECIFIED.);
#1188=B_SPLINE_SURFACE_WITH_KNOTS('',3,3,((#16798,#16799,#16800,#16801),
(#16802,#16803,#16804,#16805),(#16806,#16807,#16808,#16809),(#16810,#16811,
#16812,#16813)),.UNSPECIFIED.,.F.,.F.,.F.,(4,4),(4,4),(0.,1.),(-5.40717967697245,
-5.36678788880707),.UNSPECIFIED.);
#1189=B_SPLINE_SURFACE_WITH_KNOTS('',3,3,((#16831,#16832,#16833,#16834),
(#16835,#16836,#16837,#16838),(#16839,#16840,#16841,#16842),(#16843,#16844,
#16845,#16846)),.UNSPECIFIED.,.F.,.F.,.F.,(4,4),(4,4),(0.,1.),(-0.333212111192934,
-0.302076863348255),.UNSPECIFIED.);
#1190=B_SPLINE_SURFACE_WITH_KNOTS('',3,3,((#16856,#16857,#16858,#16859),
(#16860,#16861,#16862,#16863),(#16864,#16865,#16866,#16867),(#16868,#16869,
#16870,#16871)),.UNSPECIFIED.,.F.,.F.,.F.,(4,4),(4,4),(0.,1.),(0.,1.),
 .UNSPECIFIED.);
#1191=B_SPLINE_SURFACE_WITH_KNOTS('',3,3,((#16888,#16889,#16890,#16891),
(#16892,#16893,#16894,#16895),(#16896,#16897,#16898,#16899),(#16900,#16901,
#16902,#16903)),.UNSPECIFIED.,.F.,.F.,.F.,(4,4),(4,4),(0.,1.),(0.302076863124856,
0.333212111192934),.UNSPECIFIED.);
#1192=B_SPLINE_SURFACE_WITH_KNOTS('',3,3,((#16918,#16919,#16920,#16921),
(#16922,#16923,#16924,#16925),(#16926,#16927,#16928,#16929),(#16930,#16931,
#16932,#16933)),.UNSPECIFIED.,.F.,.F.,.F.,(4,4),(4,4),(0.,1.),(0.,1.),
 .UNSPECIFIED.);
#1193=B_SPLINE_SURFACE_WITH_KNOTS('',3,3,((#17002,#17003,#17004,#17005),
(#17006,#17007,#17008,#17009),(#17010,#17011,#17012,#17013),(#17014,#17015,
#17016,#17017)),.UNSPECIFIED.,.F.,.F.,.F.,(4,4),(4,4),(0.,1.),(0.292820323027551,
0.333212111192934),.UNSPECIFIED.);
#1194=B_SPLINE_SURFACE_WITH_KNOTS('',3,3,((#17040,#17041,#17042,#17043),
(#17044,#17045,#17046,#17047),(#17048,#17049,#17050,#17051),(#17052,#17053,
#17054,#17055)),.UNSPECIFIED.,.F.,.F.,.F.,(4,4),(4,4),(0.,1.),(5.36678788880707,
5.39792313665175),.UNSPECIFIED.);
#1195=B_SPLINE_SURFACE_WITH_KNOTS('',3,3,((#17065,#17066,#17067,#17068),
(#17069,#17070,#17071,#17072),(#17073,#17074,#17075,#17076),(#17077,#17078,
#17079,#17080)),.UNSPECIFIED.,.F.,.F.,.F.,(4,4),(4,4),(0.,1.),(0.,1.),
 .UNSPECIFIED.);
#1196=B_SPLINE_SURFACE_WITH_KNOTS('',3,3,((#17201,#17202,#17203,#17204,
#17205,#17206,#17207,#17208,#17209),(#17210,#17211,#17212,#17213,#17214,
#17215,#17216,#17217,#17218),(#17219,#17220,#17221,#17222,#17223,#17224,
#17225,#17226,#17227),(#17228,#17229,#17230,#17231,#17232,#17233,#17234,
#17235,#17236)),.UNSPECIFIED.,.F.,.F.,.F.,(4,4),(4,1,1,1,1,1,4),(0.,1.),
(0.0919588831913347,0.287428968788757,0.385164011587469,0.48289905438618,
0.580634097184891,0.678369139983603,0.776104182782314),.UNSPECIFIED.);
#1197=B_SPLINE_SURFACE_WITH_KNOTS('',3,3,((#17251,#17252,#17253,#17254,
#17255,#17256,#17257,#17258),(#17259,#17260,#17261,#17262,#17263,#17264,
#17265,#17266),(#17267,#17268,#17269,#17270,#17271,#17272,#17273,#17274),
(#17275,#17276,#17277,#17278,#17279,#17280,#17281,#17282)),
 .UNSPECIFIED.,.F.,.F.,.F.,(4,4),(4,1,1,1,1,4),(0.,1.),(0.091958883192206,
0.287428968789379,0.482899054386553,0.531766575785846,0.678369139983726,
0.776104182782313),.UNSPECIFIED.);
#1198=B_SPLINE_SURFACE_WITH_KNOTS('',3,3,((#17303,#17304,#17305,#17306,
#17307,#17308,#17309,#17310,#17311),(#17312,#17313,#17314,#17315,#17316,
#17317,#17318,#17319,#17320),(#17321,#17322,#17323,#17324,#17325,#17326,
#17327,#17328,#17329),(#17330,#17331,#17332,#17333,#17334,#17335,#17336,
#17337,#17338)),.UNSPECIFIED.,.F.,.F.,.F.,(4,4),(4,1,1,1,2,4),(0.,1.),(2.02212896015404,
2.13032466905734,2.23852037796064,2.34671608686394,2.56310750467053,2.7062742594363),
 .UNSPECIFIED.);
#1199=B_SPLINE_SURFACE_WITH_KNOTS('',3,3,((#17355,#17356,#17357,#17358),
(#17359,#17360,#17361,#17362),(#17363,#17364,#17365,#17366),(#17367,#17368,
#17369,#17370)),.UNSPECIFIED.,.F.,.F.,.F.,(4,4),(4,4),(0.,1.),(-0.333212111192934,
-0.292820323027551),.UNSPECIFIED.);
#1200=B_SPLINE_SURFACE_WITH_KNOTS('',3,3,((#17375,#17376,#17377,#17378,
#17379,#17380,#17381,#17382,#17383),(#17384,#17385,#17386,#17387,#17388,
#17389,#17390,#17391,#17392),(#17393,#17394,#17395,#17396,#17397,#17398,
#17399,#17400,#17401),(#17402,#17403,#17404,#17405,#17406,#17407,#17408,
#17409,#17410)),.UNSPECIFIED.,.F.,.F.,.F.,(4,4),(4,1,1,1,2,4),(0.,1.),(2.02212896015404,
2.13032466905734,2.23852037796064,2.34671608686394,2.56310750467053,2.70627425943714),
 .UNSPECIFIED.);
#1201=B_SPLINE_SURFACE_WITH_KNOTS('',3,3,((#17427,#17428,#17429,#17430),
(#17431,#17432,#17433,#17434),(#17435,#17436,#17437,#17438),(#17439,#17440,
#17441,#17442)),.UNSPECIFIED.,.F.,.F.,.F.,(4,4),(4,4),(0.,1.),(5.36678788880707,
5.40717967697245),.UNSPECIFIED.);
#1202=B_SPLINE_SURFACE_WITH_KNOTS('',3,3,((#17447,#17448,#17449,#17450),
(#17451,#17452,#17453,#17454),(#17455,#17456,#17457,#17458),(#17459,#17460,
#17461,#17462)),.UNSPECIFIED.,.F.,.F.,.F.,(4,4),(4,4),(0.,1.),(0.,1.),
 .UNSPECIFIED.);
#1203=B_SPLINE_SURFACE_WITH_KNOTS('',3,3,((#17467,#17468,#17469,#17470),
(#17471,#17472,#17473,#17474),(#17475,#17476,#17477,#17478),(#17479,#17480,
#17481,#17482)),.UNSPECIFIED.,.F.,.F.,.F.,(4,4),(4,4),(0.,1.),(0.,1.),
 .UNSPECIFIED.);
#1204=B_SPLINE_SURFACE_WITH_KNOTS('',3,3,((#17487,#17488,#17489,#17490),
(#17491,#17492,#17493,#17494),(#17495,#17496,#17497,#17498),(#17499,#17500,
#17501,#17502)),.UNSPECIFIED.,.F.,.F.,.F.,(4,4),(4,4),(0.,1.),(0.,1.),
 .UNSPECIFIED.);
#1205=B_SPLINE_SURFACE_WITH_KNOTS('',3,3,((#17507,#17508,#17509,#17510),
(#17511,#17512,#17513,#17514),(#17515,#17516,#17517,#17518),(#17519,#17520,
#17521,#17522)),.UNSPECIFIED.,.F.,.F.,.F.,(4,4),(4,4),(0.,1.),(0.,1.),
 .UNSPECIFIED.);
#1206=B_SPLINE_SURFACE_WITH_KNOTS('',3,3,((#18167,#18168,#18169,#18170,
#18171,#18172,#18173,#18174,#18175,#18176,#18177,#18178,#18179,#18180,#18181,
#18182,#18183,#18184,#18185,#18186,#18187,#18188,#18189,#18190,#18191,#18192,
#18193,#18194,#18195),(#18196,#18197,#18198,#18199,#18200,#18201,#18202,
#18203,#18204,#18205,#18206,#18207,#18208,#18209,#18210,#18211,#18212,#18213,
#18214,#18215,#18216,#18217,#18218,#18219,#18220,#18221,#18222,#18223,#18224),
(#18225,#18226,#18227,#18228,#18229,#18230,#18231,#18232,#18233,#18234,
#18235,#18236,#18237,#18238,#18239,#18240,#18241,#18242,#18243,#18244,#18245,
#18246,#18247,#18248,#18249,#18250,#18251,#18252,#18253),(#18254,#18255,
#18256,#18257,#18258,#18259,#18260,#18261,#18262,#18263,#18264,#18265,#18266,
#18267,#18268,#18269,#18270,#18271,#18272,#18273,#18274,#18275,#18276,#18277,
#18278,#18279,#18280,#18281,#18282)),.UNSPECIFIED.,.F.,.T.,.F.,(4,4),(4,
1,2,1,1,1,1,1,1,1,1,1,1,1,1,1,1,1,1,1,1,1,1,1,1,4),(0.,1.),(0.310721506882948,
0.387730825861464,0.464740144839981,0.573091957750491,0.600179910978118,
0.627267864205746,0.654355817433373,0.681443770661001,0.749163653730069,
0.78979558357151,0.843971490026765,0.89814739648202,0.952323302937276,1.00649920939253,
1.06067511584779,1.11485102230304,1.1690269287583,1.22320283521355,1.26383476505499,
1.33155464812406,1.35864260135169,1.38573055457932,1.41281850780694,1.43990646103457,
1.49408236748983,1.54825827394508),.UNSPECIFIED.);
#1207=B_SPLINE_SURFACE_WITH_KNOTS('',3,3,((#18453,#18454,#18455,#18456,
#18457,#18458,#18459,#18460,#18461,#18462,#18463,#18464,#18465,#18466,#18467,
#18468,#18469,#18470,#18471,#18472,#18473,#18474,#18475,#18476,#18477,#18478,
#18479,#18480),(#18481,#18482,#18483,#18484,#18485,#18486,#18487,#18488,
#18489,#18490,#18491,#18492,#18493,#18494,#18495,#18496,#18497,#18498,#18499,
#18500,#18501,#18502,#18503,#18504,#18505,#18506,#18507,#18508),(#18509,
#18510,#18511,#18512,#18513,#18514,#18515,#18516,#18517,#18518,#18519,#18520,
#18521,#18522,#18523,#18524,#18525,#18526,#18527,#18528,#18529,#18530,#18531,
#18532,#18533,#18534,#18535,#18536),(#18537,#18538,#18539,#18540,#18541,
#18542,#18543,#18544,#18545,#18546,#18547,#18548,#18549,#18550,#18551,#18552,
#18553,#18554,#18555,#18556,#18557,#18558,#18559,#18560,#18561,#18562,#18563,
#18564)),.UNSPECIFIED.,.F.,.T.,.F.,(4,4),(4,1,2,1,1,1,1,1,1,1,1,1,1,1,1,
2,2,1,1,1,1,1,4),(0.,1.),(0.930381433825624,1.00739075280414,1.08440007178266,
1.17154004903191,1.21511003765654,1.25868002628116,1.34582000353042,1.38938999215504,
1.43295998077967,1.52009995802892,1.56366994665355,1.58545494096586,1.60723993527817,
1.69437991252743,1.71616490683974,1.78151988977668,1.85897978082803,1.93621438584296,
2.01344899085789,2.03275764211163,2.05206629336536,2.09068359587282,2.16791820088776),
 .UNSPECIFIED.);
#1208=B_SPLINE_SURFACE_WITH_KNOTS('',3,3,((#18674,#18675,#18676,#18677),
(#18678,#18679,#18680,#18681),(#18682,#18683,#18684,#18685),(#18686,#18687,
#18688,#18689),(#18690,#18691,#18692,#18693),(#18694,#18695,#18696,#18697)),
 .UNSPECIFIED.,.F.,.F.,.F.,(4,1,1,4),(4,4),(0.,0.183007073635842,0.366014147271685,
0.854033010300598),(0.0593282328972054,0.895517622296388),.UNSPECIFIED.);
#1209=B_SPLINE_SURFACE_WITH_KNOTS('',3,3,((#18720,#18721,#18722,#18723),
(#18724,#18725,#18726,#18727),(#18728,#18729,#18730,#18731),(#18732,#18733,
#18734,#18735),(#18736,#18737,#18738,#18739),(#18740,#18741,#18742,#18743)),
 .UNSPECIFIED.,.F.,.F.,.F.,(4,1,1,4),(4,4),(0.147257440457363,0.512718537404208,
0.756359268702104,1.),(0.0593287707275125,0.895619345916655),
 .UNSPECIFIED.);
#1210=B_SPLINE_SURFACE_WITH_KNOTS('',3,3,((#18768,#18769,#18770,#18771),
(#18772,#18773,#18774,#18775),(#18776,#18777,#18778,#18779),(#18780,#18781,
#18782,#18783)),.UNSPECIFIED.,.F.,.F.,.F.,(4,4),(4,4),(0.,1.),(0.0638119305867456,
0.897818181014928),.UNSPECIFIED.);
#1211=B_SPLINE_SURFACE_WITH_KNOTS('',3,3,((#18813,#18814,#18815,#18816),
(#18817,#18818,#18819,#18820),(#18821,#18822,#18823,#18824),(#18825,#18826,
#18827,#18828),(#18829,#18830,#18831,#18832),(#18833,#18834,#18835,#18836)),
 .UNSPECIFIED.,.F.,.F.,.F.,(4,1,1,4),(4,4),(0.,0.183007073635851,0.366014147271702,
0.854033010300638),(0.0593282328972055,0.895517622296396),.UNSPECIFIED.);
#1212=B_SPLINE_SURFACE_WITH_KNOTS('',3,3,((#18859,#18860,#18861,#18862),
(#18863,#18864,#18865,#18866),(#18867,#18868,#18869,#18870),(#18871,#18872,
#18873,#18874),(#18875,#18876,#18877,#18878),(#18879,#18880,#18881,#18882)),
 .UNSPECIFIED.,.F.,.F.,.F.,(4,1,1,4),(4,4),(0.147257440457364,0.512718537404208,
0.756359268702104,1.),(0.0593287707275126,0.895619345916652),
 .UNSPECIFIED.);
#1213=B_SPLINE_SURFACE_WITH_KNOTS('',3,3,((#18898,#18899,#18900,#18901),
(#18902,#18903,#18904,#18905),(#18906,#18907,#18908,#18909),(#18910,#18911,
#18912,#18913)),.UNSPECIFIED.,.F.,.F.,.F.,(4,4),(4,4),(0.,1.),(0.0638119305867453,
0.897818181014928),.UNSPECIFIED.);
#1214=B_SPLINE_SURFACE_WITH_KNOTS('',3,3,((#18932,#18933,#18934,#18935),
(#18936,#18937,#18938,#18939),(#18940,#18941,#18942,#18943),(#18944,#18945,
#18946,#18947),(#18948,#18949,#18950,#18951),(#18952,#18953,#18954,#18955)),
 .UNSPECIFIED.,.F.,.F.,.F.,(4,1,1,4),(4,4),(0.,0.183007073635844,0.366014147271687,
0.854033010300603),(0.0593282328972056,0.895517622296375),.UNSPECIFIED.);
#1215=B_SPLINE_SURFACE_WITH_KNOTS('',3,3,((#18978,#18979,#18980,#18981),
(#18982,#18983,#18984,#18985),(#18986,#18987,#18988,#18989),(#18990,#18991,
#18992,#18993),(#18994,#18995,#18996,#18997),(#18998,#18999,#19000,#19001)),
 .UNSPECIFIED.,.F.,.F.,.F.,(4,1,1,4),(4,4),(0.147257440457365,0.634538903053156,
0.817269451526578,1.),(0.0593287707275126,0.895619345916675),
 .UNSPECIFIED.);
#1216=B_SPLINE_SURFACE_WITH_KNOTS('',3,3,((#19017,#19018,#19019,#19020),
(#19021,#19022,#19023,#19024),(#19025,#19026,#19027,#19028),(#19029,#19030,
#19031,#19032)),.UNSPECIFIED.,.F.,.F.,.F.,(4,4),(4,4),(0.,1.),(0.0638119305867456,
0.897818181014929),.UNSPECIFIED.);
#1217=B_SPLINE_SURFACE_WITH_KNOTS('',3,3,((#19051,#19052,#19053,#19054),
(#19055,#19056,#19057,#19058),(#19059,#19060,#19061,#19062),(#19063,#19064,
#19065,#19066),(#19067,#19068,#19069,#19070),(#19071,#19072,#19073,#19074)),
 .UNSPECIFIED.,.F.,.F.,.F.,(4,1,1,4),(4,4),(0.,0.182864493320986,0.365728986641973,
0.853367635497937),(0.0593282328972057,0.895517622296394),.UNSPECIFIED.);
#1218=B_SPLINE_SURFACE_WITH_KNOTS('',3,3,((#19097,#19098,#19099,#19100),
(#19101,#19102,#19103,#19104),(#19105,#19106,#19107,#19108),(#19109,#19110,
#19111,#19112),(#19113,#19114,#19115,#19116),(#19117,#19118,#19119,#19120)),
 .UNSPECIFIED.,.F.,.F.,.F.,(4,1,1,4),(4,4),(0.147257440457363,0.512718537404207,
0.756359268702104,1.),(0.0593287707275127,0.895619345916678),
 .UNSPECIFIED.);
#1219=B_SPLINE_SURFACE_WITH_KNOTS('',3,3,((#19136,#19137,#19138,#19139),
(#19140,#19141,#19142,#19143),(#19144,#19145,#19146,#19147),(#19148,#19149,
#19150,#19151)),.UNSPECIFIED.,.F.,.F.,.F.,(4,4),(4,4),(0.,1.),(0.0638119305867454,
0.897818181014929),.UNSPECIFIED.);
#1220=B_SPLINE_SURFACE_WITH_KNOTS('',3,3,((#19170,#19171,#19172,#19173),
(#19174,#19175,#19176,#19177),(#19178,#19179,#19180,#19181),(#19182,#19183,
#19184,#19185),(#19186,#19187,#19188,#19189),(#19190,#19191,#19192,#19193)),
 .UNSPECIFIED.,.F.,.F.,.F.,(4,1,1,4),(4,4),(0.,0.18300707363585,0.366014147271701,
0.854033010300635),(0.0593282328972055,0.895517622296389),.UNSPECIFIED.);
#1221=B_SPLINE_SURFACE_WITH_KNOTS('',3,3,((#19216,#19217,#19218,#19219),
(#19220,#19221,#19222,#19223),(#19224,#19225,#19226,#19227),(#19228,#19229,
#19230,#19231),(#19232,#19233,#19234,#19235),(#19236,#19237,#19238,#19239)),
 .UNSPECIFIED.,.F.,.F.,.F.,(4,1,1,4),(4,4),(0.146295352012394,0.512168772578511,
0.756084386289255,1.),(0.0593287707275128,0.895619345916675),
 .UNSPECIFIED.);
#1222=B_SPLINE_SURFACE_WITH_KNOTS('',3,3,((#19255,#19256,#19257,#19258),
(#19259,#19260,#19261,#19262),(#19263,#19264,#19265,#19266),(#19267,#19268,
#19269,#19270)),.UNSPECIFIED.,.F.,.F.,.F.,(4,4),(4,4),(0.,1.),(0.0638119305867453,
0.897818181014928),.UNSPECIFIED.);
#1223=B_SPLINE_SURFACE_WITH_KNOTS('',3,3,((#19289,#19290,#19291,#19292),
(#19293,#19294,#19295,#19296),(#19297,#19298,#19299,#19300),(#19301,#19302,
#19303,#19304),(#19305,#19306,#19307,#19308),(#19309,#19310,#19311,#19312)),
 .UNSPECIFIED.,.F.,.F.,.F.,(4,1,1,4),(4,4),(0.,0.183007073635854,0.366014147271708,
0.854033010300653),(0.0593282328972056,0.895517622296374),.UNSPECIFIED.);
#1224=B_SPLINE_SURFACE_WITH_KNOTS('',3,3,((#19335,#19336,#19337,#19338),
(#19339,#19340,#19341,#19342),(#19343,#19344,#19345,#19346),(#19347,#19348,
#19349,#19350),(#19351,#19352,#19353,#19354),(#19355,#19356,#19357,#19358)),
 .UNSPECIFIED.,.F.,.F.,.F.,(4,1,1,4),(4,4),(0.147257440457363,0.512718537404207,
0.756359268702104,1.),(0.0593287707275127,0.895619345916681),
 .UNSPECIFIED.);
#1225=B_SPLINE_SURFACE_WITH_KNOTS('',3,3,((#19374,#19375,#19376,#19377),
(#19378,#19379,#19380,#19381),(#19382,#19383,#19384,#19385),(#19386,#19387,
#19388,#19389)),.UNSPECIFIED.,.F.,.F.,.F.,(4,4),(4,4),(0.,1.),(0.0638119305867453,
0.897818181014928),.UNSPECIFIED.);
#1226=B_SPLINE_SURFACE_WITH_KNOTS('',3,3,((#19408,#19409,#19410,#19411),
(#19412,#19413,#19414,#19415),(#19416,#19417,#19418,#19419),(#19420,#19421,
#19422,#19423),(#19424,#19425,#19426,#19427),(#19428,#19429,#19430,#19431)),
 .UNSPECIFIED.,.F.,.F.,.F.,(4,1,1,4),(4,4),(0.,0.183007073635845,0.36601414727169,
0.854033010300609),(0.0593282328972055,0.895517622296379),.UNSPECIFIED.);
#1227=B_SPLINE_SURFACE_WITH_KNOTS('',3,3,((#19454,#19455,#19456,#19457),
(#19458,#19459,#19460,#19461),(#19462,#19463,#19464,#19465),(#19466,#19467,
#19468,#19469),(#19470,#19471,#19472,#19473),(#19474,#19475,#19476,#19477)),
 .UNSPECIFIED.,.F.,.F.,.F.,(4,1,1,4),(4,4),(0.147257440457364,0.512718537404208,
0.756359268702104,1.),(0.0593287707275128,0.895619345916639),
 .UNSPECIFIED.);
#1228=B_SPLINE_SURFACE_WITH_KNOTS('',3,3,((#19493,#19494,#19495,#19496),
(#19497,#19498,#19499,#19500),(#19501,#19502,#19503,#19504),(#19505,#19506,
#19507,#19508)),.UNSPECIFIED.,.F.,.F.,.F.,(4,4),(4,4),(0.,1.),(0.0638119305867455,
0.897818181014928),.UNSPECIFIED.);
#1229=B_SPLINE_SURFACE_WITH_KNOTS('',3,3,((#19527,#19528,#19529,#19530),
(#19531,#19532,#19533,#19534),(#19535,#19536,#19537,#19538),(#19539,#19540,
#19541,#19542),(#19543,#19544,#19545,#19546),(#19547,#19548,#19549,#19550)),
 .UNSPECIFIED.,.F.,.F.,.F.,(4,1,1,4),(4,4),(0.,0.18300707363585,0.3660141472717,
0.854033010300634),(0.0593282328972057,0.895517622296377),.UNSPECIFIED.);
#1230=B_SPLINE_SURFACE_WITH_KNOTS('',3,3,((#19573,#19574,#19575,#19576),
(#19577,#19578,#19579,#19580),(#19581,#19582,#19583,#19584),(#19585,#19586,
#19587,#19588),(#19589,#19590,#19591,#19592),(#19593,#19594,#19595,#19596)),
 .UNSPECIFIED.,.F.,.F.,.F.,(4,1,1,4),(4,4),(0.147257440457363,0.634538903053156,
0.817269451526578,1.),(0.0593287707275124,0.895619345916661),
 .UNSPECIFIED.);
#1231=B_SPLINE_SURFACE_WITH_KNOTS('',3,3,((#19612,#19613,#19614,#19615),
(#19616,#19617,#19618,#19619),(#19620,#19621,#19622,#19623),(#19624,#19625,
#19626,#19627)),.UNSPECIFIED.,.F.,.F.,.F.,(4,4),(4,4),(0.,1.),(0.0638119305867453,
0.897818181014928),.UNSPECIFIED.);
#1232=B_SPLINE_SURFACE_WITH_KNOTS('',3,3,((#19646,#19647,#19648,#19649),
(#19650,#19651,#19652,#19653),(#19654,#19655,#19656,#19657),(#19658,#19659,
#19660,#19661),(#19662,#19663,#19664,#19665),(#19666,#19667,#19668,#19669)),
 .UNSPECIFIED.,.F.,.F.,.F.,(4,1,1,4),(4,4),(0.,0.182864493320987,0.365728986641974,
0.853367635497938),(0.0593282328972058,0.895517622296391),.UNSPECIFIED.);
#1233=B_SPLINE_SURFACE_WITH_KNOTS('',3,3,((#19692,#19693,#19694,#19695),
(#19696,#19697,#19698,#19699),(#19700,#19701,#19702,#19703),(#19704,#19705,
#19706,#19707),(#19708,#19709,#19710,#19711),(#19712,#19713,#19714,#19715)),
 .UNSPECIFIED.,.F.,.F.,.F.,(4,1,1,4),(4,4),(0.147257440457363,0.634538903053156,
0.817269451526578,1.),(0.059328770727513,0.895619345916667),
 .UNSPECIFIED.);
#1234=B_SPLINE_SURFACE_WITH_KNOTS('',3,3,((#19731,#19732,#19733,#19734),
(#19735,#19736,#19737,#19738),(#19739,#19740,#19741,#19742),(#19743,#19744,
#19745,#19746)),.UNSPECIFIED.,.F.,.F.,.F.,(4,4),(4,4),(0.,1.),(0.0638119305867456,
0.897818181014928),.UNSPECIFIED.);
#1235=B_SPLINE_SURFACE_WITH_KNOTS('',3,3,((#19765,#19766,#19767,#19768),
(#19769,#19770,#19771,#19772),(#19773,#19774,#19775,#19776),(#19777,#19778,
#19779,#19780),(#19781,#19782,#19783,#19784),(#19785,#19786,#19787,#19788)),
 .UNSPECIFIED.,.F.,.F.,.F.,(4,1,1,4),(4,4),(0.,0.183007073635851,0.366014147271702,
0.854033010300638),(0.0593282328972056,0.895517622296395),.UNSPECIFIED.);
#1236=B_SPLINE_SURFACE_WITH_KNOTS('',3,3,((#19816,#19817,#19818,#19819),
(#19820,#19821,#19822,#19823),(#19824,#19825,#19826,#19827),(#19828,#19829,
#19830,#19831),(#19832,#19833,#19834,#19835),(#19836,#19837,#19838,#19839)),
 .UNSPECIFIED.,.F.,.F.,.F.,(4,1,1,4),(4,4),(0.146295352012395,0.512168772578511,
0.756084386289256,1.),(0.0593287707275127,0.895619345916662),
 .UNSPECIFIED.);
#1237=B_SPLINE_SURFACE_WITH_KNOTS('',3,3,((#19855,#19856,#19857,#19858),
(#19859,#19860,#19861,#19862),(#19863,#19864,#19865,#19866),(#19867,#19868,
#19869,#19870)),.UNSPECIFIED.,.F.,.F.,.F.,(4,4),(4,4),(0.,1.),(0.0638119305867453,
0.897818181014928),.UNSPECIFIED.);
#1238=B_SPLINE_SURFACE_WITH_KNOTS('',3,3,((#19889,#19890,#19891,#19892),
(#19893,#19894,#19895,#19896),(#19897,#19898,#19899,#19900),(#19901,#19902,
#19903,#19904),(#19905,#19906,#19907,#19908),(#19909,#19910,#19911,#19912)),
 .UNSPECIFIED.,.F.,.F.,.F.,(4,1,1,4),(4,4),(0.,0.18300707363585,0.3660141472717,
0.854033010300633),(0.0593282328972056,0.895517622296402),.UNSPECIFIED.);
#1239=B_SPLINE_SURFACE_WITH_KNOTS('',3,3,((#19935,#19936,#19937,#19938),
(#19939,#19940,#19941,#19942),(#19943,#19944,#19945,#19946),(#19947,#19948,
#19949,#19950),(#19951,#19952,#19953,#19954),(#19955,#19956,#19957,#19958)),
 .UNSPECIFIED.,.F.,.F.,.F.,(4,1,1,4),(4,4),(0.147257440457363,0.512718537404207,
0.756359268702104,1.),(0.0593287707275125,0.895619345916659),
 .UNSPECIFIED.);
#1240=B_SPLINE_SURFACE_WITH_KNOTS('',3,3,((#19974,#19975,#19976,#19977),
(#19978,#19979,#19980,#19981),(#19982,#19983,#19984,#19985),(#19986,#19987,
#19988,#19989)),.UNSPECIFIED.,.F.,.F.,.F.,(4,4),(4,4),(0.,1.),(0.0638119305867455,
0.897818181014928),.UNSPECIFIED.);
#1241=B_SPLINE_SURFACE_WITH_KNOTS('',3,3,((#20008,#20009,#20010,#20011),
(#20012,#20013,#20014,#20015),(#20016,#20017,#20018,#20019),(#20020,#20021,
#20022,#20023),(#20024,#20025,#20026,#20027),(#20028,#20029,#20030,#20031)),
 .UNSPECIFIED.,.F.,.F.,.F.,(4,1,1,4),(4,4),(0.,0.183007073635855,0.366014147271709,
0.854033010300655),(0.0593282328972057,0.895517622296379),.UNSPECIFIED.);
#1242=B_SPLINE_SURFACE_WITH_KNOTS('',3,3,((#20054,#20055,#20056,#20057),
(#20058,#20059,#20060,#20061),(#20062,#20063,#20064,#20065),(#20066,#20067,
#20068,#20069),(#20070,#20071,#20072,#20073),(#20074,#20075,#20076,#20077)),
 .UNSPECIFIED.,.F.,.F.,.F.,(4,1,1,4),(4,4),(0.147257440457364,0.512718537404208,
0.756359268702104,1.),(0.0593287707275129,0.895619345916649),
 .UNSPECIFIED.);
#1243=B_SPLINE_SURFACE_WITH_KNOTS('',3,3,((#20093,#20094,#20095,#20096),
(#20097,#20098,#20099,#20100),(#20101,#20102,#20103,#20104),(#20105,#20106,
#20107,#20108)),.UNSPECIFIED.,.F.,.F.,.F.,(4,4),(4,4),(0.,1.),(0.0638119305867455,
0.897818181014929),.UNSPECIFIED.);
#1244=B_SPLINE_SURFACE_WITH_KNOTS('',3,3,((#20127,#20128,#20129,#20130),
(#20131,#20132,#20133,#20134),(#20135,#20136,#20137,#20138),(#20139,#20140,
#20141,#20142),(#20143,#20144,#20145,#20146),(#20147,#20148,#20149,#20150)),
 .UNSPECIFIED.,.F.,.F.,.F.,(4,1,1,4),(4,4),(0.,0.183007073635856,0.366014147271713,
0.854033010300663),(0.0593282328972055,0.895517622296378),.UNSPECIFIED.);
#1245=B_SPLINE_SURFACE_WITH_KNOTS('',3,3,((#20173,#20174,#20175,#20176),
(#20177,#20178,#20179,#20180),(#20181,#20182,#20183,#20184),(#20185,#20186,
#20187,#20188),(#20189,#20190,#20191,#20192),(#20193,#20194,#20195,#20196)),
 .UNSPECIFIED.,.F.,.F.,.F.,(4,1,1,4),(4,4),(0.147257440457363,0.512718537404207,
0.756359268702104,1.),(0.0593287707275125,0.895619345916676),
 .UNSPECIFIED.);
#1246=B_SPLINE_SURFACE_WITH_KNOTS('',3,3,((#20212,#20213,#20214,#20215),
(#20216,#20217,#20218,#20219),(#20220,#20221,#20222,#20223),(#20224,#20225,
#20226,#20227)),.UNSPECIFIED.,.F.,.F.,.F.,(4,4),(4,4),(0.,1.),(0.0638119305867453,
0.897818181014928),.UNSPECIFIED.);
#1247=B_SPLINE_SURFACE_WITH_KNOTS('',3,3,((#20246,#20247,#20248,#20249),
(#20250,#20251,#20252,#20253),(#20254,#20255,#20256,#20257),(#20258,#20259,
#20260,#20261),(#20262,#20263,#20264,#20265),(#20266,#20267,#20268,#20269)),
 .UNSPECIFIED.,.F.,.F.,.F.,(4,1,1,4),(4,4),(0.,0.243819324427982,0.487638648855963,
0.853367635497936),(0.0593282328972057,0.895517622296394),.UNSPECIFIED.);
#1248=B_SPLINE_SURFACE_WITH_KNOTS('',3,3,((#20292,#20293,#20294,#20295),
(#20296,#20297,#20298,#20299),(#20300,#20301,#20302,#20303),(#20304,#20305,
#20306,#20307),(#20308,#20309,#20310,#20311),(#20312,#20313,#20314,#20315)),
 .UNSPECIFIED.,.F.,.F.,.F.,(4,1,1,4),(4,4),(0.147257440457363,0.512718537404207,
0.756359268702104,1.),(0.0593287707275129,0.895619345916666),
 .UNSPECIFIED.);
#1249=B_SPLINE_SURFACE_WITH_KNOTS('',3,3,((#20331,#20332,#20333,#20334),
(#20335,#20336,#20337,#20338),(#20339,#20340,#20341,#20342),(#20343,#20344,
#20345,#20346)),.UNSPECIFIED.,.F.,.F.,.F.,(4,4),(4,4),(0.,1.),(0.0638119305867456,
0.897818181014929),.UNSPECIFIED.);
#1250=B_SPLINE_SURFACE_WITH_KNOTS('',3,3,((#20365,#20366,#20367,#20368),
(#20369,#20370,#20371,#20372),(#20373,#20374,#20375,#20376),(#20377,#20378,
#20379,#20380),(#20381,#20382,#20383,#20384),(#20385,#20386,#20387,#20388)),
 .UNSPECIFIED.,.F.,.F.,.F.,(4,1,1,4),(4,4),(0.,0.183007073635844,0.366014147271688,
0.854033010300606),(0.0593282328972055,0.895517622296384),.UNSPECIFIED.);
#1251=B_SPLINE_SURFACE_WITH_KNOTS('',3,3,((#20411,#20412,#20413,#20414),
(#20415,#20416,#20417,#20418),(#20419,#20420,#20421,#20422),(#20423,#20424,
#20425,#20426),(#20427,#20428,#20429,#20430),(#20431,#20432,#20433,#20434)),
 .UNSPECIFIED.,.F.,.F.,.F.,(4,1,1,4),(4,4),(0.146295352012395,0.634126579433884,
0.817063289716942,1.),(0.0593287707275129,0.895619345916667),
 .UNSPECIFIED.);
#1252=B_SPLINE_SURFACE_WITH_KNOTS('',3,3,((#20450,#20451,#20452,#20453),
(#20454,#20455,#20456,#20457),(#20458,#20459,#20460,#20461),(#20462,#20463,
#20464,#20465)),.UNSPECIFIED.,.F.,.F.,.F.,(4,4),(4,4),(0.,1.),(0.0638119305867452,
0.897818181014929),.UNSPECIFIED.);
#1253=B_SPLINE_SURFACE_WITH_KNOTS('',3,3,((#20484,#20485,#20486,#20487),
(#20488,#20489,#20490,#20491),(#20492,#20493,#20494,#20495),(#20496,#20497,
#20498,#20499),(#20500,#20501,#20502,#20503),(#20504,#20505,#20506,#20507)),
 .UNSPECIFIED.,.F.,.F.,.F.,(4,1,1,4),(4,4),(0.,0.183007073635857,0.366014147271714,
0.854033010300667),(0.0593282328972057,0.895517622296367),.UNSPECIFIED.);
#1254=B_SPLINE_SURFACE_WITH_KNOTS('',3,3,((#20530,#20531,#20532,#20533),
(#20534,#20535,#20536,#20537),(#20538,#20539,#20540,#20541),(#20542,#20543,
#20544,#20545),(#20546,#20547,#20548,#20549),(#20550,#20551,#20552,#20553)),
 .UNSPECIFIED.,.F.,.F.,.F.,(4,1,1,4),(4,4),(0.147257440457363,0.512718537404208,
0.756359268702104,1.),(0.0593287707275124,0.89561934591667),
 .UNSPECIFIED.);
#1255=B_SPLINE_SURFACE_WITH_KNOTS('',3,3,((#20569,#20570,#20571,#20572),
(#20573,#20574,#20575,#20576),(#20577,#20578,#20579,#20580),(#20581,#20582,
#20583,#20584)),.UNSPECIFIED.,.F.,.F.,.F.,(4,4),(4,4),(0.,1.),(0.063811930586745,
0.897818181014928),.UNSPECIFIED.);
#1256=B_SPLINE_SURFACE_WITH_KNOTS('',3,3,((#20603,#20604,#20605,#20606),
(#20607,#20608,#20609,#20610),(#20611,#20612,#20613,#20614),(#20615,#20616,
#20617,#20618),(#20619,#20620,#20621,#20622),(#20623,#20624,#20625,#20626)),
 .UNSPECIFIED.,.F.,.F.,.F.,(4,1,1,4),(4,4),(0.,0.18300707363585,0.3660141472717,
0.854033010300632),(0.0593282328972055,0.895517622296395),.UNSPECIFIED.);
#1257=B_SPLINE_SURFACE_WITH_KNOTS('',3,3,((#20649,#20650,#20651,#20652),
(#20653,#20654,#20655,#20656),(#20657,#20658,#20659,#20660),(#20661,#20662,
#20663,#20664),(#20665,#20666,#20667,#20668),(#20669,#20670,#20671,#20672)),
 .UNSPECIFIED.,.F.,.F.,.F.,(4,1,1,4),(4,4),(0.147257440457364,0.634538903053156,
0.817269451526578,1.),(0.0593287707275127,0.895619345916657),
 .UNSPECIFIED.);
#1258=B_SPLINE_SURFACE_WITH_KNOTS('',3,3,((#20688,#20689,#20690,#20691),
(#20692,#20693,#20694,#20695),(#20696,#20697,#20698,#20699),(#20700,#20701,
#20702,#20703)),.UNSPECIFIED.,.F.,.F.,.F.,(4,4),(4,4),(0.,1.),(0.0638119305867455,
0.897818181014928),.UNSPECIFIED.);
#1259=B_SPLINE_SURFACE_WITH_KNOTS('',3,3,((#20722,#20723,#20724,#20725),
(#20726,#20727,#20728,#20729),(#20730,#20731,#20732,#20733),(#20734,#20735,
#20736,#20737),(#20738,#20739,#20740,#20741),(#20742,#20743,#20744,#20745)),
 .UNSPECIFIED.,.F.,.F.,.F.,(4,1,1,4),(4,4),(0.,0.183007073635853,0.366014147271705,
0.854033010300645),(0.0593282328972057,0.895517622296384),.UNSPECIFIED.);
#1260=B_SPLINE_SURFACE_WITH_KNOTS('',3,3,((#20768,#20769,#20770,#20771),
(#20772,#20773,#20774,#20775),(#20776,#20777,#20778,#20779),(#20780,#20781,
#20782,#20783),(#20784,#20785,#20786,#20787),(#20788,#20789,#20790,#20791)),
 .UNSPECIFIED.,.F.,.F.,.F.,(4,1,1,4),(4,4),(0.147257440457364,0.512718537404208,
0.756359268702104,1.),(0.0593287707275128,0.895619345916678),
 .UNSPECIFIED.);
#1261=B_SPLINE_SURFACE_WITH_KNOTS('',3,3,((#20807,#20808,#20809,#20810),
(#20811,#20812,#20813,#20814),(#20815,#20816,#20817,#20818),(#20819,#20820,
#20821,#20822)),.UNSPECIFIED.,.F.,.F.,.F.,(4,4),(4,4),(0.,1.),(0.0638119305867456,
0.897818181014929),.UNSPECIFIED.);
#1262=B_SPLINE_SURFACE_WITH_KNOTS('',3,3,((#20841,#20842,#20843,#20844),
(#20845,#20846,#20847,#20848),(#20849,#20850,#20851,#20852),(#20853,#20854,
#20855,#20856),(#20857,#20858,#20859,#20860),(#20861,#20862,#20863,#20864)),
 .UNSPECIFIED.,.F.,.F.,.F.,(4,1,1,4),(4,4),(0.147257440457363,0.634538903053156,
0.817269451526578,1.),(0.0593287707275126,0.895619345916645),
 .UNSPECIFIED.);
#1263=B_SPLINE_SURFACE_WITH_KNOTS('',3,3,((#20880,#20881,#20882,#20883),
(#20884,#20885,#20886,#20887),(#20888,#20889,#20890,#20891),(#20892,#20893,
#20894,#20895)),.UNSPECIFIED.,.F.,.F.,.F.,(4,4),(4,4),(0.,1.),(0.0638119305867452,
0.897818181014928),.UNSPECIFIED.);
#1264=B_SPLINE_SURFACE_WITH_KNOTS('',3,3,((#20910,#20911,#20912,#20913),
(#20914,#20915,#20916,#20917),(#20918,#20919,#20920,#20921),(#20922,#20923,
#20924,#20925),(#20926,#20927,#20928,#20929),(#20930,#20931,#20932,#20933)),
 .UNSPECIFIED.,.F.,.F.,.F.,(4,1,1,4),(4,4),(0.,0.243819324427982,0.487638648855964,
0.853367635497937),(0.0593282328972056,0.895517622296376),.UNSPECIFIED.);
#1265=B_SPLINE_SURFACE_WITH_KNOTS('',3,3,((#20949,#20950,#20951,#20952),
(#20953,#20954,#20955,#20956),(#20957,#20958,#20959,#20960),(#20961,#20962,
#20963,#20964),(#20965,#20966,#20967,#20968),(#20969,#20970,#20971,#20972)),
 .UNSPECIFIED.,.F.,.F.,.F.,(4,1,1,4),(4,4),(0.146295352012396,0.634126579433884,
0.817063289716942,1.),(0.059328770727513,0.895619345916653),
 .UNSPECIFIED.);
#1266=B_SPLINE_SURFACE_WITH_KNOTS('',3,3,((#20997,#20998,#20999,#21000),
(#21001,#21002,#21003,#21004),(#21005,#21006,#21007,#21008),(#21009,#21010,
#21011,#21012)),.UNSPECIFIED.,.F.,.F.,.F.,(4,4),(4,4),(0.,1.),(0.0638119305867454,
0.897818181014928),.UNSPECIFIED.);
#1267=B_SPLINE_SURFACE_WITH_KNOTS('',3,3,((#21027,#21028,#21029,#21030),
(#21031,#21032,#21033,#21034),(#21035,#21036,#21037,#21038),(#21039,#21040,
#21041,#21042),(#21043,#21044,#21045,#21046),(#21047,#21048,#21049,#21050)),
 .UNSPECIFIED.,.F.,.F.,.F.,(4,1,1,4),(4,4),(0.,0.183007073635845,0.366014147271691,
0.854033010300612),(0.0593282328972056,0.89551762229639),.UNSPECIFIED.);
#1268=B_SPLINE_SURFACE_WITH_KNOTS('',3,3,((#21152,#21153,#21154,#21155,
#21156,#21157,#21158,#21159,#21160,#21161,#21162,#21163,#21164,#21165,#21166,
#21167,#21168,#21169,#21170,#21171,#21172,#21173,#21174,#21175,#21176,#21177,
#21178,#21179,#21180),(#21181,#21182,#21183,#21184,#21185,#21186,#21187,
#21188,#21189,#21190,#21191,#21192,#21193,#21194,#21195,#21196,#21197,#21198,
#21199,#21200,#21201,#21202,#21203,#21204,#21205,#21206,#21207,#21208,#21209),
(#21210,#21211,#21212,#21213,#21214,#21215,#21216,#21217,#21218,#21219,
#21220,#21221,#21222,#21223,#21224,#21225,#21226,#21227,#21228,#21229,#21230,
#21231,#21232,#21233,#21234,#21235,#21236,#21237,#21238),(#21239,#21240,
#21241,#21242,#21243,#21244,#21245,#21246,#21247,#21248,#21249,#21250,#21251,
#21252,#21253,#21254,#21255,#21256,#21257,#21258,#21259,#21260,#21261,#21262,
#21263,#21264,#21265,#21266,#21267)),.UNSPECIFIED.,.F.,.T.,.F.,(4,4),(4,
1,2,1,1,1,1,1,1,1,1,1,1,1,1,1,1,1,1,1,1,1,1,1,1,4),(0.,1.),(0.310721506882948,
0.387730825861464,0.464740144839981,0.573091957750491,0.600179910978118,
0.627267864205746,0.654355817433373,0.681443770661001,0.749163653730069,
0.78979558357151,0.843971490026765,0.89814739648202,0.952323302937276,1.00649920939253,
1.06067511584779,1.11485102230304,1.1690269287583,1.22320283521355,1.26383476505499,
1.33155464812406,1.35864260135169,1.38573055457932,1.41281850780694,1.43990646103457,
1.49408236748983,1.54825827394508),.UNSPECIFIED.);
#1269=B_SPLINE_SURFACE_WITH_KNOTS('',3,3,((#21478,#21479,#21480,#21481,
#21482,#21483,#21484,#21485,#21486,#21487,#21488,#21489,#21490,#21491,#21492,
#21493,#21494,#21495,#21496,#21497,#21498,#21499,#21500,#21501,#21502,#21503,
#21504,#21505),(#21506,#21507,#21508,#21509,#21510,#21511,#21512,#21513,
#21514,#21515,#21516,#21517,#21518,#21519,#21520,#21521,#21522,#21523,#21524,
#21525,#21526,#21527,#21528,#21529,#21530,#21531,#21532,#21533),(#21534,
#21535,#21536,#21537,#21538,#21539,#21540,#21541,#21542,#21543,#21544,#21545,
#21546,#21547,#21548,#21549,#21550,#21551,#21552,#21553,#21554,#21555,#21556,
#21557,#21558,#21559,#21560,#21561),(#21562,#21563,#21564,#21565,#21566,
#21567,#21568,#21569,#21570,#21571,#21572,#21573,#21574,#21575,#21576,#21577,
#21578,#21579,#21580,#21581,#21582,#21583,#21584,#21585,#21586,#21587,#21588,
#21589)),.UNSPECIFIED.,.F.,.T.,.F.,(4,4),(4,1,2,1,1,1,1,1,1,1,1,1,1,1,1,
2,2,1,1,1,1,1,4),(0.,1.),(0.930381433825624,1.00739075280414,1.08440007178266,
1.17154004903191,1.21511003765654,1.25868002628116,1.34582000353042,1.38938999215504,
1.43295998077967,1.52009995802892,1.56366994665355,1.58545494096586,1.60723993527817,
1.69437991252743,1.71616490683974,1.78151988977668,1.85897978082803,1.93621438584296,
2.01344899085789,2.03275764211163,2.05206629336536,2.09068359587282,2.16791820088776),
 .UNSPECIFIED.);
#1270=B_SPLINE_SURFACE_WITH_KNOTS('',3,3,((#21736,#21737,#21738,#21739),
(#21740,#21741,#21742,#21743),(#21744,#21745,#21746,#21747),(#21748,#21749,
#21750,#21751),(#21752,#21753,#21754,#21755),(#21756,#21757,#21758,#21759)),
 .UNSPECIFIED.,.F.,.F.,.F.,(4,1,1,4),(4,4),(0.,0.243643268493762,0.487286536987524,
0.852751439728166),(0.0593287711114826,0.89552230135485),.UNSPECIFIED.);
#1271=B_SPLINE_SURFACE_WITH_KNOTS('',3,3,((#21792,#21793,#21794,#21795),
(#21796,#21797,#21798,#21799),(#21800,#21801,#21802,#21803),(#21804,#21805,
#21806,#21807),(#21808,#21809,#21810,#21811),(#21812,#21813,#21814,#21815)),
 .UNSPECIFIED.,.F.,.F.,.F.,(4,1,1,4),(4,4),(0.145114332397141,0.511493904226938,
0.755746952113469,1.),(0.0593282329032902,0.895635080262268),
 .UNSPECIFIED.);
#1272=B_SPLINE_SURFACE_WITH_KNOTS('',3,3,((#21848,#21849,#21850,#21851),
(#21852,#21853,#21854,#21855),(#21856,#21857,#21858,#21859),(#21860,#21861,
#21862,#21863)),.UNSPECIFIED.,.F.,.F.,.F.,(4,4),(4,4),(0.,1.),(0.0638119305867453,
0.897818175643156),.UNSPECIFIED.);
#1273=B_SPLINE_SURFACE_WITH_KNOTS('',3,3,((#22404,#22405,#22406,#22407),
(#22408,#22409,#22410,#22411),(#22412,#22413,#22414,#22415),(#22416,#22417,
#22418,#22419),(#22420,#22421,#22422,#22423),(#22424,#22425,#22426,#22427)),
 .UNSPECIFIED.,.F.,.F.,.F.,(4,1,1,4),(4,4),(0.,0.182732451370321,0.365464902740643,
0.852751439728166),(0.0593287711114824,0.895522301354867),.UNSPECIFIED.);
#1274=B_SPLINE_SURFACE_WITH_KNOTS('',3,3,((#22450,#22451,#22452,#22453),
(#22454,#22455,#22456,#22457),(#22458,#22459,#22460,#22461),(#22462,#22463,
#22464,#22465),(#22466,#22467,#22468,#22469),(#22470,#22471,#22472,#22473)),
 .UNSPECIFIED.,.F.,.F.,.F.,(4,1,1,4),(4,4),(0.145491947870824,0.63378226337321,
0.816891131686605,1.),(0.0593282329020183,0.895635080262244),
 .UNSPECIFIED.);
#1275=B_SPLINE_SURFACE_WITH_KNOTS('',3,3,((#22489,#22490,#22491,#22492),
(#22493,#22494,#22495,#22496),(#22497,#22498,#22499,#22500),(#22501,#22502,
#22503,#22504)),.UNSPECIFIED.,.F.,.F.,.F.,(4,4),(4,4),(0.,1.),(0.0638119305867452,
0.897818175643156),.UNSPECIFIED.);
#1276=B_SPLINE_SURFACE_WITH_KNOTS('',3,3,((#22523,#22524,#22525,#22526),
(#22527,#22528,#22529,#22530),(#22531,#22532,#22533,#22534),(#22535,#22536,
#22537,#22538),(#22539,#22540,#22541,#22542),(#22543,#22544,#22545,#22546)),
 .UNSPECIFIED.,.F.,.F.,.F.,(4,1,1,4),(4,4),(0.,0.182732451370321,0.365464902740643,
0.852751439728167),(0.0593287711114828,0.895522301354858),.UNSPECIFIED.);
#1277=B_SPLINE_SURFACE_WITH_KNOTS('',3,3,((#22569,#22570,#22571,#22572),
(#22573,#22574,#22575,#22576),(#22577,#22578,#22579,#22580),(#22581,#22582,
#22583,#22584),(#22585,#22586,#22587,#22588),(#22589,#22590,#22591,#22592)),
 .UNSPECIFIED.,.F.,.F.,.F.,(4,1,1,4),(4,4),(0.145491947870788,0.633782263373195,
0.816891131686597,1.),(0.0593282329020185,0.89563508026229),
 .UNSPECIFIED.);
#1278=B_SPLINE_SURFACE_WITH_KNOTS('',3,3,((#22608,#22609,#22610,#22611),
(#22612,#22613,#22614,#22615),(#22616,#22617,#22618,#22619),(#22620,#22621,
#22622,#22623)),.UNSPECIFIED.,.F.,.F.,.F.,(4,4),(4,4),(0.,1.),(0.0638119305867454,
0.897818175643156),.UNSPECIFIED.);
#1279=B_SPLINE_SURFACE_WITH_KNOTS('',3,3,((#22642,#22643,#22644,#22645),
(#22646,#22647,#22648,#22649),(#22650,#22651,#22652,#22653),(#22654,#22655,
#22656,#22657),(#22658,#22659,#22660,#22661),(#22662,#22663,#22664,#22665)),
 .UNSPECIFIED.,.F.,.F.,.F.,(4,1,1,4),(4,4),(0.,0.182732451370321,0.365464902740643,
0.852751439728166),(0.0593287711114824,0.895522301354853),.UNSPECIFIED.);
#1280=B_SPLINE_SURFACE_WITH_KNOTS('',3,3,((#22688,#22689,#22690,#22691),
(#22692,#22693,#22694,#22695),(#22696,#22697,#22698,#22699),(#22700,#22701,
#22702,#22703),(#22704,#22705,#22706,#22707),(#22708,#22709,#22710,#22711)),
 .UNSPECIFIED.,.F.,.F.,.F.,(4,1,1,4),(4,4),(0.145491947870791,0.633782263373196,
0.816891131686598,1.),(0.0593282329020185,0.895635080262257),
 .UNSPECIFIED.);
#1281=B_SPLINE_SURFACE_WITH_KNOTS('',3,3,((#22727,#22728,#22729,#22730),
(#22731,#22732,#22733,#22734),(#22735,#22736,#22737,#22738),(#22739,#22740,
#22741,#22742)),.UNSPECIFIED.,.F.,.F.,.F.,(4,4),(4,4),(0.,1.),(0.0638119305867454,
0.897818175643157),.UNSPECIFIED.);
#1282=B_SPLINE_SURFACE_WITH_KNOTS('',3,3,((#22761,#22762,#22763,#22764),
(#22765,#22766,#22767,#22768),(#22769,#22770,#22771,#22772),(#22773,#22774,
#22775,#22776),(#22777,#22778,#22779,#22780),(#22781,#22782,#22783,#22784)),
 .UNSPECIFIED.,.F.,.F.,.F.,(4,1,1,4),(4,4),(0.,0.243691231740892,0.487382463481784,
0.852919311093121),(0.0593287711114826,0.895503416457802),.UNSPECIFIED.);
#1283=B_SPLINE_SURFACE_WITH_KNOTS('',3,3,((#22807,#22808,#22809,#22810),
(#22811,#22812,#22813,#22814),(#22815,#22816,#22817,#22818),(#22819,#22820,
#22821,#22822),(#22823,#22824,#22825,#22826),(#22827,#22828,#22829,#22830)),
 .UNSPECIFIED.,.F.,.F.,.F.,(4,1,1,4),(4,4),(0.145491947870838,0.511709684497622,
0.755854842248811,1.),(0.0593282329020186,0.895635080262274),
 .UNSPECIFIED.);
#1284=B_SPLINE_SURFACE_WITH_KNOTS('',3,3,((#22846,#22847,#22848,#22849),
(#22850,#22851,#22852,#22853),(#22854,#22855,#22856,#22857),(#22858,#22859,
#22860,#22861)),.UNSPECIFIED.,.F.,.F.,.F.,(4,4),(4,4),(0.,1.),(0.0638119305867452,
0.897818175643157),.UNSPECIFIED.);
#1285=B_SPLINE_SURFACE_WITH_KNOTS('',3,3,((#22880,#22881,#22882,#22883),
(#22884,#22885,#22886,#22887),(#22888,#22889,#22890,#22891),(#22892,#22893,
#22894,#22895),(#22896,#22897,#22898,#22899),(#22900,#22901,#22902,#22903)),
 .UNSPECIFIED.,.F.,.F.,.F.,(4,1,1,4),(4,4),(0.,0.182732451370321,0.365464902740643,
0.852751439728166),(0.0593287711114825,0.895522301354848),.UNSPECIFIED.);
#1286=B_SPLINE_SURFACE_WITH_KNOTS('',3,3,((#22926,#22927,#22928,#22929),
(#22930,#22931,#22932,#22933),(#22934,#22935,#22936,#22937),(#22938,#22939,
#22940,#22941),(#22942,#22943,#22944,#22945),(#22946,#22947,#22948,#22949)),
 .UNSPECIFIED.,.F.,.F.,.F.,(4,1,1,4),(4,4),(0.145114332397166,0.511493904226952,
0.755746952113476,1.),(0.0593282329032902,0.895635080262249),
 .UNSPECIFIED.);
#1287=B_SPLINE_SURFACE_WITH_KNOTS('',3,3,((#22965,#22966,#22967,#22968),
(#22969,#22970,#22971,#22972),(#22973,#22974,#22975,#22976),(#22977,#22978,
#22979,#22980)),.UNSPECIFIED.,.F.,.F.,.F.,(4,4),(4,4),(0.,1.),(0.0638119305867454,
0.897818175643156),.UNSPECIFIED.);
#1288=B_SPLINE_SURFACE_WITH_KNOTS('',3,3,((#22999,#23000,#23001,#23002),
(#23003,#23004,#23005,#23006),(#23007,#23008,#23009,#23010),(#23011,#23012,
#23013,#23014),(#23015,#23016,#23017,#23018),(#23019,#23020,#23021,#23022)),
 .UNSPECIFIED.,.F.,.F.,.F.,(4,1,1,4),(4,4),(0.,0.182732451370321,0.365464902740642,
0.852751439728166),(0.0593287711114824,0.895522301354846),.UNSPECIFIED.);
#1289=B_SPLINE_SURFACE_WITH_KNOTS('',3,3,((#23045,#23046,#23047,#23048),
(#23049,#23050,#23051,#23052),(#23053,#23054,#23055,#23056),(#23057,#23058,
#23059,#23060),(#23061,#23062,#23063,#23064),(#23065,#23066,#23067,#23068)),
 .UNSPECIFIED.,.F.,.F.,.F.,(4,1,1,4),(4,4),(0.145491947870832,0.511709684497618,
0.755854842248809,1.),(0.0593282329020186,0.895635080262275),
 .UNSPECIFIED.);
#1290=B_SPLINE_SURFACE_WITH_KNOTS('',3,3,((#23084,#23085,#23086,#23087),
(#23088,#23089,#23090,#23091),(#23092,#23093,#23094,#23095),(#23096,#23097,
#23098,#23099)),.UNSPECIFIED.,.F.,.F.,.F.,(4,4),(4,4),(0.,1.),(0.0638119305867453,
0.897818175643157),.UNSPECIFIED.);
#1291=B_SPLINE_SURFACE_WITH_KNOTS('',3,3,((#23118,#23119,#23120,#23121),
(#23122,#23123,#23124,#23125),(#23126,#23127,#23128,#23129),(#23130,#23131,
#23132,#23133),(#23134,#23135,#23136,#23137),(#23138,#23139,#23140,#23141)),
 .UNSPECIFIED.,.F.,.F.,.F.,(4,1,1,4),(4,4),(0.,0.243643268493762,0.487286536987524,
0.852751439728166),(0.0593287711114823,0.895522301354865),.UNSPECIFIED.);
#1292=B_SPLINE_SURFACE_WITH_KNOTS('',3,3,((#23164,#23165,#23166,#23167),
(#23168,#23169,#23170,#23171),(#23172,#23173,#23174,#23175),(#23176,#23177,
#23178,#23179),(#23180,#23181,#23182,#23183),(#23184,#23185,#23186,#23187)),
 .UNSPECIFIED.,.F.,.F.,.F.,(4,1,1,4),(4,4),(0.145491947870811,0.633782263373205,
0.816891131686602,1.),(0.0593282329020184,0.895635080262268),
 .UNSPECIFIED.);
#1293=B_SPLINE_SURFACE_WITH_KNOTS('',3,3,((#23203,#23204,#23205,#23206),
(#23207,#23208,#23209,#23210),(#23211,#23212,#23213,#23214),(#23215,#23216,
#23217,#23218)),.UNSPECIFIED.,.F.,.F.,.F.,(4,4),(4,4),(0.,1.),(0.0638119305867452,
0.897818175643156),.UNSPECIFIED.);
#1294=B_SPLINE_SURFACE_WITH_KNOTS('',3,3,((#23237,#23238,#23239,#23240),
(#23241,#23242,#23243,#23244),(#23245,#23246,#23247,#23248),(#23249,#23250,
#23251,#23252),(#23253,#23254,#23255,#23256),(#23257,#23258,#23259,#23260)),
 .UNSPECIFIED.,.F.,.F.,.F.,(4,1,1,4),(4,4),(0.,0.182732451370321,0.365464902740643,
0.852751439728167),(0.0593287711114826,0.895522301354835),.UNSPECIFIED.);
#1295=B_SPLINE_SURFACE_WITH_KNOTS('',3,3,((#23283,#23284,#23285,#23286),
(#23287,#23288,#23289,#23290),(#23291,#23292,#23293,#23294),(#23295,#23296,
#23297,#23298),(#23299,#23300,#23301,#23302),(#23303,#23304,#23305,#23306)),
 .UNSPECIFIED.,.F.,.F.,.F.,(4,1,1,4),(4,4),(0.145491947870803,0.511709684497601,
0.755854842248801,1.),(0.0593282329020183,0.895635080262279),
 .UNSPECIFIED.);
#1296=B_SPLINE_SURFACE_WITH_KNOTS('',3,3,((#23322,#23323,#23324,#23325),
(#23326,#23327,#23328,#23329),(#23330,#23331,#23332,#23333),(#23334,#23335,
#23336,#23337)),.UNSPECIFIED.,.F.,.F.,.F.,(4,4),(4,4),(0.,1.),(0.063811930586745,
0.897818175643157),.UNSPECIFIED.);
#1297=B_SPLINE_SURFACE_WITH_KNOTS('',3,3,((#23356,#23357,#23358,#23359),
(#23360,#23361,#23362,#23363),(#23364,#23365,#23366,#23367),(#23368,#23369,
#23370,#23371),(#23372,#23373,#23374,#23375),(#23376,#23377,#23378,#23379)),
 .UNSPECIFIED.,.F.,.F.,.F.,(4,1,1,4),(4,4),(0.,0.182768423805669,0.365536847611337,
0.852919311093121),(0.0593287711114827,0.895503416457805),.UNSPECIFIED.);
#1298=B_SPLINE_SURFACE_WITH_KNOTS('',3,3,((#23402,#23403,#23404,#23405),
(#23406,#23407,#23408,#23409),(#23410,#23411,#23412,#23413),(#23414,#23415,
#23416,#23417),(#23418,#23419,#23420,#23421),(#23422,#23423,#23424,#23425)),
 .UNSPECIFIED.,.F.,.F.,.F.,(4,1,1,4),(4,4),(0.145491947870775,0.511709684497586,
0.755854842248793,1.),(0.0593282329020186,0.895635080262287),
 .UNSPECIFIED.);
#1299=B_SPLINE_SURFACE_WITH_KNOTS('',3,3,((#23446,#23447,#23448,#23449),
(#23450,#23451,#23452,#23453),(#23454,#23455,#23456,#23457),(#23458,#23459,
#23460,#23461)),.UNSPECIFIED.,.F.,.F.,.F.,(4,4),(4,4),(0.,1.),(0.0638119305867453,
0.897818175643156),.UNSPECIFIED.);
#1300=B_SPLINE_SURFACE_WITH_KNOTS('',3,3,((#23480,#23481,#23482,#23483),
(#23484,#23485,#23486,#23487),(#23488,#23489,#23490,#23491),(#23492,#23493,
#23494,#23495),(#23496,#23497,#23498,#23499),(#23500,#23501,#23502,#23503)),
 .UNSPECIFIED.,.F.,.F.,.F.,(4,1,1,4),(4,4),(0.,0.182732451370321,0.365464902740643,
0.852751439728167),(0.0593287711114827,0.895522301354846),.UNSPECIFIED.);
#1301=B_SPLINE_SURFACE_WITH_KNOTS('',3,3,((#23526,#23527,#23528,#23529),
(#23530,#23531,#23532,#23533),(#23534,#23535,#23536,#23537),(#23538,#23539,
#23540,#23541),(#23542,#23543,#23544,#23545),(#23546,#23547,#23548,#23549)),
 .UNSPECIFIED.,.F.,.F.,.F.,(4,1,1,4),(4,4),(0.145114332397139,0.511493904226937,
0.755746952113468,1.),(0.0593282329032903,0.895635080262252),
 .UNSPECIFIED.);
#1302=B_SPLINE_SURFACE_WITH_KNOTS('',3,3,((#23565,#23566,#23567,#23568),
(#23569,#23570,#23571,#23572),(#23573,#23574,#23575,#23576),(#23577,#23578,
#23579,#23580)),.UNSPECIFIED.,.F.,.F.,.F.,(4,4),(4,4),(0.,1.),(0.0638119305867454,
0.897818175643156),.UNSPECIFIED.);
#1303=B_SPLINE_SURFACE_WITH_KNOTS('',3,3,((#23599,#23600,#23601,#23602),
(#23603,#23604,#23605,#23606),(#23607,#23608,#23609,#23610),(#23611,#23612,
#23613,#23614),(#23615,#23616,#23617,#23618),(#23619,#23620,#23621,#23622)),
 .UNSPECIFIED.,.F.,.F.,.F.,(4,1,1,4),(4,4),(0.,0.182732451370321,0.365464902740643,
0.852751439728166),(0.0593287711114825,0.895522301354846),.UNSPECIFIED.);
#1304=B_SPLINE_SURFACE_WITH_KNOTS('',3,3,((#23645,#23646,#23647,#23648),
(#23649,#23650,#23651,#23652),(#23653,#23654,#23655,#23656),(#23657,#23658,
#23659,#23660),(#23661,#23662,#23663,#23664),(#23665,#23666,#23667,#23668)),
 .UNSPECIFIED.,.F.,.F.,.F.,(4,1,1,4),(4,4),(0.145491947870806,0.511709684497604,
0.755854842248802,1.),(0.0593282329020184,0.895635080262275),
 .UNSPECIFIED.);
#1305=B_SPLINE_SURFACE_WITH_KNOTS('',3,3,((#23684,#23685,#23686,#23687),
(#23688,#23689,#23690,#23691),(#23692,#23693,#23694,#23695),(#23696,#23697,
#23698,#23699)),.UNSPECIFIED.,.F.,.F.,.F.,(4,4),(4,4),(0.,1.),(0.0638119305867451,
0.897818175643157),.UNSPECIFIED.);
#1306=B_SPLINE_SURFACE_WITH_KNOTS('',3,3,((#23718,#23719,#23720,#23721),
(#23722,#23723,#23724,#23725),(#23726,#23727,#23728,#23729),(#23730,#23731,
#23732,#23733),(#23734,#23735,#23736,#23737),(#23738,#23739,#23740,#23741)),
 .UNSPECIFIED.,.F.,.F.,.F.,(4,1,1,4),(4,4),(0.,0.243643268493762,0.487286536987524,
0.852751439728167),(0.0593287711114822,0.895522301354865),.UNSPECIFIED.);
#1307=B_SPLINE_SURFACE_WITH_KNOTS('',3,3,((#23764,#23765,#23766,#23767),
(#23768,#23769,#23770,#23771),(#23772,#23773,#23774,#23775),(#23776,#23777,
#23778,#23779),(#23780,#23781,#23782,#23783),(#23784,#23785,#23786,#23787)),
 .UNSPECIFIED.,.F.,.F.,.F.,(4,1,1,4),(4,4),(0.14549194787082,0.633782263373209,
0.816891131686604,1.),(0.0593282329020183,0.895635080262269),
 .UNSPECIFIED.);
#1308=B_SPLINE_SURFACE_WITH_KNOTS('',3,3,((#23803,#23804,#23805,#23806),
(#23807,#23808,#23809,#23810),(#23811,#23812,#23813,#23814),(#23815,#23816,
#23817,#23818)),.UNSPECIFIED.,.F.,.F.,.F.,(4,4),(4,4),(0.,1.),(0.0638119305867451,
0.897818175643156),.UNSPECIFIED.);
#1309=B_SPLINE_SURFACE_WITH_KNOTS('',3,3,((#23837,#23838,#23839,#23840),
(#23841,#23842,#23843,#23844),(#23845,#23846,#23847,#23848),(#23849,#23850,
#23851,#23852),(#23853,#23854,#23855,#23856),(#23857,#23858,#23859,#23860)),
 .UNSPECIFIED.,.F.,.F.,.F.,(4,1,1,4),(4,4),(0.,0.182732451370321,0.365464902740643,
0.852751439728167),(0.0593287711114825,0.895522301354872),.UNSPECIFIED.);
#1310=B_SPLINE_SURFACE_WITH_KNOTS('',3,3,((#23883,#23884,#23885,#23886),
(#23887,#23888,#23889,#23890),(#23891,#23892,#23893,#23894),(#23895,#23896,
#23897,#23898),(#23899,#23900,#23901,#23902),(#23903,#23904,#23905,#23906)),
 .UNSPECIFIED.,.F.,.F.,.F.,(4,1,1,4),(4,4),(0.145491947870777,0.511709684497587,
0.755854842248793,1.),(0.0593282329020184,0.895635080262259),
 .UNSPECIFIED.);
#1311=B_SPLINE_SURFACE_WITH_KNOTS('',3,3,((#23922,#23923,#23924,#23925),
(#23926,#23927,#23928,#23929),(#23930,#23931,#23932,#23933),(#23934,#23935,
#23936,#23937)),.UNSPECIFIED.,.F.,.F.,.F.,(4,4),(4,4),(0.,1.),(0.0638119305867454,
0.897818175643156),.UNSPECIFIED.);
#1312=B_SPLINE_SURFACE_WITH_KNOTS('',3,3,((#23956,#23957,#23958,#23959),
(#23960,#23961,#23962,#23963),(#23964,#23965,#23966,#23967),(#23968,#23969,
#23970,#23971),(#23972,#23973,#23974,#23975),(#23976,#23977,#23978,#23979)),
 .UNSPECIFIED.,.F.,.F.,.F.,(4,1,1,4),(4,4),(0.,0.182768423805668,0.365536847611337,
0.852919311093119),(0.0593287711114823,0.895503416457802),.UNSPECIFIED.);
#1313=B_SPLINE_SURFACE_WITH_KNOTS('',3,3,((#24002,#24003,#24004,#24005),
(#24006,#24007,#24008,#24009),(#24010,#24011,#24012,#24013),(#24014,#24015,
#24016,#24017),(#24018,#24019,#24020,#24021),(#24022,#24023,#24024,#24025)),
 .UNSPECIFIED.,.F.,.F.,.F.,(4,1,1,4),(4,4),(0.145491947870815,0.511709684497608,
0.755854842248804,1.),(0.0593282329020187,0.895635080262285),
 .UNSPECIFIED.);
#1314=B_SPLINE_SURFACE_WITH_KNOTS('',3,3,((#24041,#24042,#24043,#24044),
(#24045,#24046,#24047,#24048),(#24049,#24050,#24051,#24052),(#24053,#24054,
#24055,#24056)),.UNSPECIFIED.,.F.,.F.,.F.,(4,4),(4,4),(0.,1.),(0.0638119305867453,
0.897818175643157),.UNSPECIFIED.);
#1315=B_SPLINE_SURFACE_WITH_KNOTS('',3,3,((#24075,#24076,#24077,#24078),
(#24079,#24080,#24081,#24082),(#24083,#24084,#24085,#24086),(#24087,#24088,
#24089,#24090),(#24091,#24092,#24093,#24094),(#24095,#24096,#24097,#24098)),
 .UNSPECIFIED.,.F.,.F.,.F.,(4,1,1,4),(4,4),(0.,0.182732451370321,0.365464902740643,
0.852751439728166),(0.0593287711114823,0.895522301354835),.UNSPECIFIED.);
#1316=B_SPLINE_SURFACE_WITH_KNOTS('',3,3,((#24121,#24122,#24123,#24124),
(#24125,#24126,#24127,#24128),(#24129,#24130,#24131,#24132),(#24133,#24134,
#24135,#24136),(#24137,#24138,#24139,#24140),(#24141,#24142,#24143,#24144)),
 .UNSPECIFIED.,.F.,.F.,.F.,(4,1,1,4),(4,4),(0.145114332397162,0.51149390422695,
0.755746952113475,1.),(0.0593282329032904,0.895635080262261),
 .UNSPECIFIED.);
#1317=B_SPLINE_SURFACE_WITH_KNOTS('',3,3,((#24160,#24161,#24162,#24163),
(#24164,#24165,#24166,#24167),(#24168,#24169,#24170,#24171),(#24172,#24173,
#24174,#24175)),.UNSPECIFIED.,.F.,.F.,.F.,(4,4),(4,4),(0.,1.),(0.0638119305867451,
0.897818175643156),.UNSPECIFIED.);
#1318=B_SPLINE_SURFACE_WITH_KNOTS('',3,3,((#24194,#24195,#24196,#24197),
(#24198,#24199,#24200,#24201),(#24202,#24203,#24204,#24205),(#24206,#24207,
#24208,#24209),(#24210,#24211,#24212,#24213),(#24214,#24215,#24216,#24217)),
 .UNSPECIFIED.,.F.,.F.,.F.,(4,1,1,4),(4,4),(0.,0.182732451370321,0.365464902740642,
0.852751439728166),(0.0593287711114828,0.895522301354838),.UNSPECIFIED.);
#1319=B_SPLINE_SURFACE_WITH_KNOTS('',3,3,((#24240,#24241,#24242,#24243),
(#24244,#24245,#24246,#24247),(#24248,#24249,#24250,#24251),(#24252,#24253,
#24254,#24255),(#24256,#24257,#24258,#24259),(#24260,#24261,#24262,#24263)),
 .UNSPECIFIED.,.F.,.F.,.F.,(4,1,1,4),(4,4),(0.1454919478708,0.5117096844976,
0.7558548422488,1.),(0.0593282329020184,0.895635080262241),
 .UNSPECIFIED.);
#1320=B_SPLINE_SURFACE_WITH_KNOTS('',3,3,((#24279,#24280,#24281,#24282),
(#24283,#24284,#24285,#24286),(#24287,#24288,#24289,#24290),(#24291,#24292,
#24293,#24294)),.UNSPECIFIED.,.F.,.F.,.F.,(4,4),(4,4),(0.,1.),(0.0638119305867454,
0.897818175643156),.UNSPECIFIED.);
#1321=B_SPLINE_SURFACE_WITH_KNOTS('',3,3,((#24313,#24314,#24315,#24316),
(#24317,#24318,#24319,#24320),(#24321,#24322,#24323,#24324),(#24325,#24326,
#24327,#24328),(#24329,#24330,#24331,#24332),(#24333,#24334,#24335,#24336)),
 .UNSPECIFIED.,.F.,.F.,.F.,(4,1,1,4),(4,4),(0.,0.182732451370321,0.365464902740643,
0.852751439728166),(0.0593287711114826,0.895522301354858),.UNSPECIFIED.);
#1322=B_SPLINE_SURFACE_WITH_KNOTS('',3,3,((#24359,#24360,#24361,#24362),
(#24363,#24364,#24365,#24366),(#24367,#24368,#24369,#24370),(#24371,#24372,
#24373,#24374),(#24375,#24376,#24377,#24378),(#24379,#24380,#24381,#24382)),
 .UNSPECIFIED.,.F.,.F.,.F.,(4,1,1,4),(4,4),(0.145491947870816,0.511709684497609,
0.755854842248805,1.),(0.0593282329020187,0.89563508026227),
 .UNSPECIFIED.);
#1323=B_SPLINE_SURFACE_WITH_KNOTS('',3,3,((#24398,#24399,#24400,#24401),
(#24402,#24403,#24404,#24405),(#24406,#24407,#24408,#24409),(#24410,#24411,
#24412,#24413)),.UNSPECIFIED.,.F.,.F.,.F.,(4,4),(4,4),(0.,1.),(0.0638119305867453,
0.897818175643156),.UNSPECIFIED.);
#1324=B_SPLINE_SURFACE_WITH_KNOTS('',3,3,((#24432,#24433,#24434,#24435),
(#24436,#24437,#24438,#24439),(#24440,#24441,#24442,#24443),(#24444,#24445,
#24446,#24447),(#24448,#24449,#24450,#24451),(#24452,#24453,#24454,#24455)),
 .UNSPECIFIED.,.F.,.F.,.F.,(4,1,1,4),(4,4),(0.145491947870804,0.511709684497602,
0.755854842248801,1.),(0.0593282329020183,0.895635080262241),
 .UNSPECIFIED.);
#1325=B_SPLINE_SURFACE_WITH_KNOTS('',3,3,((#24471,#24472,#24473,#24474),
(#24475,#24476,#24477,#24478),(#24479,#24480,#24481,#24482),(#24483,#24484,
#24485,#24486)),.UNSPECIFIED.,.F.,.F.,.F.,(4,4),(4,4),(0.,1.),(0.0638119305867451,
0.897818175643156),.UNSPECIFIED.);
#1326=B_SPLINE_SURFACE_WITH_KNOTS('',3,3,((#24501,#24502,#24503,#24504),
(#24505,#24506,#24507,#24508),(#24509,#24510,#24511,#24512),(#24513,#24514,
#24515,#24516),(#24517,#24518,#24519,#24520),(#24521,#24522,#24523,#24524)),
 .UNSPECIFIED.,.F.,.F.,.F.,(4,1,1,4),(4,4),(0.,0.182732451370321,0.365464902740643,
0.852751439728167),(0.0593287711114822,0.895522301354863),.UNSPECIFIED.);
#1327=B_SPLINE_SURFACE_WITH_KNOTS('',3,3,((#24540,#24541,#24542,#24543),
(#24544,#24545,#24546,#24547),(#24548,#24549,#24550,#24551),(#24552,#24553,
#24554,#24555),(#24556,#24557,#24558,#24559),(#24560,#24561,#24562,#24563)),
 .UNSPECIFIED.,.F.,.F.,.F.,(4,1,1,4),(4,4),(0.145491947870802,0.633782263373201,
0.8168911316866,1.),(0.0593282329020185,0.895635080262271),
 .UNSPECIFIED.);
#1328=B_SPLINE_SURFACE_WITH_KNOTS('',3,3,((#24588,#24589,#24590,#24591),
(#24592,#24593,#24594,#24595),(#24596,#24597,#24598,#24599),(#24600,#24601,
#24602,#24603)),.UNSPECIFIED.,.F.,.F.,.F.,(4,4),(4,4),(0.,1.),(0.0638119305867454,
0.897818175643156),.UNSPECIFIED.);
#1329=B_SPLINE_SURFACE_WITH_KNOTS('',3,3,((#24618,#24619,#24620,#24621),
(#24622,#24623,#24624,#24625),(#24626,#24627,#24628,#24629),(#24630,#24631,
#24632,#24633),(#24634,#24635,#24636,#24637),(#24638,#24639,#24640,#24641)),
 .UNSPECIFIED.,.F.,.F.,.F.,(4,1,1,4),(4,4),(0.,0.182767788823199,0.365535577646398,
0.852916347841596),(0.0593287711114826,0.895503517333978),.UNSPECIFIED.);
#1330=B_SPLINE_SURFACE_WITH_KNOTS('',3,3,((#26368,#26369,#26370,#26371,
#26372,#26373,#26374,#26375,#26376,#26377,#26378,#26379,#26380,#26381,#26382,
#26383,#26384,#26385,#26386,#26387,#26388,#26389,#26390,#26391,#26392,#26393,
#26394,#26395,#26396,#26397,#26398,#26399,#26400,#26401,#26402,#26403,#26404,
#26405,#26406,#26407,#26408,#26409),(#26410,#26411,#26412,#26413,#26414,
#26415,#26416,#26417,#26418,#26419,#26420,#26421,#26422,#26423,#26424,#26425,
#26426,#26427,#26428,#26429,#26430,#26431,#26432,#26433,#26434,#26435,#26436,
#26437,#26438,#26439,#26440,#26441,#26442,#26443,#26444,#26445,#26446,#26447,
#26448,#26449,#26450,#26451),(#26452,#26453,#26454,#26455,#26456,#26457,
#26458,#26459,#26460,#26461,#26462,#26463,#26464,#26465,#26466,#26467,#26468,
#26469,#26470,#26471,#26472,#26473,#26474,#26475,#26476,#26477,#26478,#26479,
#26480,#26481,#26482,#26483,#26484,#26485,#26486,#26487,#26488,#26489,#26490,
#26491,#26492,#26493),(#26494,#26495,#26496,#26497,#26498,#26499,#26500,
#26501,#26502,#26503,#26504,#26505,#26506,#26507,#26508,#26509,#26510,#26511,
#26512,#26513,#26514,#26515,#26516,#26517,#26518,#26519,#26520,#26521,#26522,
#26523,#26524,#26525,#26526,#26527,#26528,#26529,#26530,#26531,#26532,#26533,
#26534,#26535)),.UNSPECIFIED.,.F.,.F.,.F.,(4,4),(4,1,1,1,1,1,1,1,1,1,1,
1,1,1,1,1,1,1,1,1,1,1,1,1,1,1,1,1,1,1,1,1,1,1,1,1,1,1,1,4),(0.,0.0460148164544131),
(8.31058692273978,9.29381890460478,10.2770508864698,11.2602828683348,12.2435148501998,
13.2267468320648,14.2099788139298,15.1932107957948,16.1764427776598,17.1596747595248,
18.1429067413898,19.1261387232548,20.1093707051198,21.0926026869848,22.0758346688498,
23.0590666507148,24.0422986325798,25.0255306144448,26.0087625963098,26.9919945781748,
27.9752265600398,28.9584585419048,29.9416905237698,30.9249225056348,31.9081544874998,
32.8913864693648,33.8746184512298,34.8578504330948,35.8410824149598,36.8243143968248,
37.8075463786898,38.7907783605548,39.7740103424198,40.7572423242848,41.7404743061498,
42.7237062880148,43.7069382698798,44.6901702517448,45.6734022336098,46.6566342154749),
 .UNSPECIFIED.);
#1331=B_SPLINE_SURFACE_WITH_KNOTS('',3,3,((#26681,#26682,#26683,#26684,
#26685,#26686,#26687,#26688,#26689,#26690,#26691,#26692,#26693,#26694,#26695,
#26696,#26697,#26698,#26699,#26700,#26701,#26702,#26703,#26704,#26705,#26706,
#26707,#26708,#26709,#26710,#26711,#26712,#26713,#26714,#26715,#26716,#26717,
#26718,#26719,#26720,#26721,#26722),(#26723,#26724,#26725,#26726,#26727,
#26728,#26729,#26730,#26731,#26732,#26733,#26734,#26735,#26736,#26737,#26738,
#26739,#26740,#26741,#26742,#26743,#26744,#26745,#26746,#26747,#26748,#26749,
#26750,#26751,#26752,#26753,#26754,#26755,#26756,#26757,#26758,#26759,#26760,
#26761,#26762,#26763,#26764),(#26765,#26766,#26767,#26768,#26769,#26770,
#26771,#26772,#26773,#26774,#26775,#26776,#26777,#26778,#26779,#26780,#26781,
#26782,#26783,#26784,#26785,#26786,#26787,#26788,#26789,#26790,#26791,#26792,
#26793,#26794,#26795,#26796,#26797,#26798,#26799,#26800,#26801,#26802,#26803,
#26804,#26805,#26806),(#26807,#26808,#26809,#26810,#26811,#26812,#26813,
#26814,#26815,#26816,#26817,#26818,#26819,#26820,#26821,#26822,#26823,#26824,
#26825,#26826,#26827,#26828,#26829,#26830,#26831,#26832,#26833,#26834,#26835,
#26836,#26837,#26838,#26839,#26840,#26841,#26842,#26843,#26844,#26845,#26846,
#26847,#26848)),.UNSPECIFIED.,.F.,.F.,.F.,(4,4),(4,1,1,1,1,1,1,1,1,1,1,
1,1,1,1,1,1,1,1,1,1,1,1,1,1,1,1,1,1,1,1,1,1,1,1,1,1,1,1,4),(0.,0.0460148164544132),
(11.6154215191106,12.5986535009756,13.5818854828406,14.5651174647056,15.5483494465706,
16.5315814284356,17.5148134103006,18.4980453921656,19.4812773740306,20.4645093558957,
21.4477413377607,22.4309733196257,23.4142053014907,24.3974372833557,25.3806692652207,
26.3639012470857,27.3471332289507,28.3303652108157,29.3135971926807,30.2968291745457,
31.2800611564107,32.2632931382757,33.2465251201407,34.2297571020057,35.2129890838707,
36.1962210657357,37.1794530476007,38.1626850294657,39.1459170113307,40.1291489931957,
41.1123809750607,42.0956129569257,43.0788449387907,44.0620769206557,45.0453089025207,
46.0285408843857,47.0117728662507,47.9950048481157,48.9782368299807,49.9614688118457),
 .UNSPECIFIED.);
#1332=B_SPLINE_SURFACE_WITH_KNOTS('',3,3,((#28645,#28646,#28647,#28648,
#28649,#28650,#28651,#28652,#28653,#28654,#28655,#28656,#28657,#28658,#28659,
#28660,#28661,#28662,#28663,#28664,#28665,#28666,#28667,#28668,#28669,#28670,
#28671,#28672,#28673,#28674,#28675,#28676,#28677,#28678,#28679,#28680,#28681,
#28682,#28683,#28684,#28685,#28686,#28687,#28688,#28689,#28690,#28691,#28692,
#28693,#28694,#28695,#28696,#28697,#28698,#28699,#28700,#28701,#28702,#28703,
#28704,#28705,#28706,#28707,#28708,#28709,#28710,#28711,#28712,#28713,#28714,
#28715,#28716,#28717,#28718,#28719,#28720,#28721,#28722,#28723,#28724,#28725,
#28726,#28727,#28728,#28729,#28730,#28731,#28732,#28733,#28734,#28735,#28736,
#28737,#28738,#28739,#28740,#28741,#28742,#28743,#28744,#28745,#28746,#28747,
#28748,#28749,#28750,#28751,#28752,#28753,#28754,#28755,#28756,#28757,#28758,
#28759,#28760,#28761,#28762,#28763,#28764,#28765,#28766,#28767,#28768,#28769,
#28770,#28771,#28772,#28773,#28774,#28775,#28776,#28777,#28778,#28779,#28780,
#28781,#28782,#28783,#28784,#28785,#28786,#28787,#28788,#28789,#28790,#28791,
#28792,#28793,#28794,#28795,#28796,#28797,#28798),(#28799,#28800,#28801,
#28802,#28803,#28804,#28805,#28806,#28807,#28808,#28809,#28810,#28811,#28812,
#28813,#28814,#28815,#28816,#28817,#28818,#28819,#28820,#28821,#28822,#28823,
#28824,#28825,#28826,#28827,#28828,#28829,#28830,#28831,#28832,#28833,#28834,
#28835,#28836,#28837,#28838,#28839,#28840,#28841,#28842,#28843,#28844,#28845,
#28846,#28847,#28848,#28849,#28850,#28851,#28852,#28853,#28854,#28855,#28856,
#28857,#28858,#28859,#28860,#28861,#28862,#28863,#28864,#28865,#28866,#28867,
#28868,#28869,#28870,#28871,#28872,#28873,#28874,#28875,#28876,#28877,#28878,
#28879,#28880,#28881,#28882,#28883,#28884,#28885,#28886,#28887,#28888,#28889,
#28890,#28891,#28892,#28893,#28894,#28895,#28896,#28897,#28898,#28899,#28900,
#28901,#28902,#28903,#28904,#28905,#28906,#28907,#28908,#28909,#28910,#28911,
#28912,#28913,#28914,#28915,#28916,#28917,#28918,#28919,#28920,#28921,#28922,
#28923,#28924,#28925,#28926,#28927,#28928,#28929,#28930,#28931,#28932,#28933,
#28934,#28935,#28936,#28937,#28938,#28939,#28940,#28941,#28942,#28943,#28944,
#28945,#28946,#28947,#28948,#28949,#28950,#28951,#28952),(#28953,#28954,
#28955,#28956,#28957,#28958,#28959,#28960,#28961,#28962,#28963,#28964,#28965,
#28966,#28967,#28968,#28969,#28970,#28971,#28972,#28973,#28974,#28975,#28976,
#28977,#28978,#28979,#28980,#28981,#28982,#28983,#28984,#28985,#28986,#28987,
#28988,#28989,#28990,#28991,#28992,#28993,#28994,#28995,#28996,#28997,#28998,
#28999,#29000,#29001,#29002,#29003,#29004,#29005,#29006,#29007,#29008,#29009,
#29010,#29011,#29012,#29013,#29014,#29015,#29016,#29017,#29018,#29019,#29020,
#29021,#29022,#29023,#29024,#29025,#29026,#29027,#29028,#29029,#29030,#29031,
#29032,#29033,#29034,#29035,#29036,#29037,#29038,#29039,#29040,#29041,#29042,
#29043,#29044,#29045,#29046,#29047,#29048,#29049,#29050,#29051,#29052,#29053,
#29054,#29055,#29056,#29057,#29058,#29059,#29060,#29061,#29062,#29063,#29064,
#29065,#29066,#29067,#29068,#29069,#29070,#29071,#29072,#29073,#29074,#29075,
#29076,#29077,#29078,#29079,#29080,#29081,#29082,#29083,#29084,#29085,#29086,
#29087,#29088,#29089,#29090,#29091,#29092,#29093,#29094,#29095,#29096,#29097,
#29098,#29099,#29100,#29101,#29102,#29103,#29104,#29105,#29106),(#29107,
#29108,#29109,#29110,#29111,#29112,#29113,#29114,#29115,#29116,#29117,#29118,
#29119,#29120,#29121,#29122,#29123,#29124,#29125,#29126,#29127,#29128,#29129,
#29130,#29131,#29132,#29133,#29134,#29135,#29136,#29137,#29138,#29139,#29140,
#29141,#29142,#29143,#29144,#29145,#29146,#29147,#29148,#29149,#29150,#29151,
#29152,#29153,#29154,#29155,#29156,#29157,#29158,#29159,#29160,#29161,#29162,
#29163,#29164,#29165,#29166,#29167,#29168,#29169,#29170,#29171,#29172,#29173,
#29174,#29175,#29176,#29177,#29178,#29179,#29180,#29181,#29182,#29183,#29184,
#29185,#29186,#29187,#29188,#29189,#29190,#29191,#29192,#29193,#29194,#29195,
#29196,#29197,#29198,#29199,#29200,#29201,#29202,#29203,#29204,#29205,#29206,
#29207,#29208,#29209,#29210,#29211,#29212,#29213,#29214,#29215,#29216,#29217,
#29218,#29219,#29220,#29221,#29222,#29223,#29224,#29225,#29226,#29227,#29228,
#29229,#29230,#29231,#29232,#29233,#29234,#29235,#29236,#29237,#29238,#29239,
#29240,#29241,#29242,#29243,#29244,#29245,#29246,#29247,#29248,#29249,#29250,
#29251,#29252,#29253,#29254,#29255,#29256,#29257,#29258,#29259,#29260)),
 .UNSPECIFIED.,.F.,.F.,.F.,(4,4),(4,1,1,1,1,1,1,1,1,1,1,1,1,1,1,1,1,1,1,
1,1,1,1,1,1,1,1,1,1,1,1,1,1,1,1,1,1,1,1,1,1,1,1,1,1,1,1,1,1,1,1,1,1,1,1,
1,1,1,1,1,1,1,1,1,1,1,1,1,1,1,1,1,1,1,1,1,1,1,1,1,1,1,1,1,1,1,1,1,1,1,1,
1,1,1,1,1,1,1,1,1,1,1,1,1,1,1,1,1,1,1,1,1,1,1,1,1,1,1,1,1,1,1,1,1,1,1,1,
1,1,1,1,1,1,1,1,1,1,1,1,1,1,1,1,1,1,1,1,1,1,1,1,4),(0.,0.0658467982010769),
(8.30747755240111,9.30559832175319,10.3037190911053,11.3018398604573,12.2999606298094,
13.2980813991615,14.2962021685136,15.2943229378657,16.2924437072177,17.2905644765698,
18.2886852459219,19.286806015274,20.2849267846261,21.2830475539781,22.2811683233302,
23.2792890926823,24.2774098620344,25.2755306313865,26.2736514007385,27.2717721700906,
28.2698929394427,29.2680137087948,30.2661344781468,31.2642552474989,32.262376016851,
33.2604967862031,34.2586175555552,35.2567383249072,36.2548590942593,37.2529798636114,
38.2511006329635,39.2492214023156,40.2473421716676,41.2454629410197,42.2435837103718,
43.2417044797239,44.2398252490759,45.237946018428,46.2360667877801,47.2341875571322,
48.2323083264843,49.2304290958363,50.2285498651884,51.2266706345405,52.2247914038926,
53.2229121732447,54.2210329425967,55.2191537119488,56.2172744813009,57.215395250653,
58.213516020005,59.2116367893571,60.2097575587092,61.2078783280613,62.2059990974134,
63.2041198667654,64.2022406361175,65.2003614054696,66.1984821748217,67.1966029441738,
68.1947237135258,69.1928444828779,70.19096525223,71.1890860215821,72.1872067909342,
73.1853275602862,74.1834483296383,75.1815690989904,76.1796898683425,77.1778106376945,
78.1759314070466,79.1740521763987,80.1721729457508,81.1702937151029,82.1684144844549,
83.166535253807,84.1646560231591,85.1627767925112,86.1608975618633,87.1590183312153,
88.1571391005674,89.1552598699195,90.1533806392716,91.1515014086236,92.1496221779757,
93.1477429473278,94.1458637166799,95.143984486032,96.142105255384,97.1402260247361,
98.1383467940882,99.1364675634403,100.134588332792,101.132709102144,102.130829871497,
103.128950640849,104.127071410201,105.125192179553,106.123312948905,107.121433718257,
108.119554487609,109.117675256961,110.115796026313,111.113916795665,112.112037565017,
113.110158334369,114.108279103721,115.106399873074,116.104520642426,117.102641411778,
118.10076218113,119.098882950482,120.097003719834,121.095124489186,122.093245258538,
123.09136602789,124.089486797242,125.087607566594,126.085728335946,127.083849105298,
128.081969874651,129.080090644003,130.078211413355,131.076332182707,132.074452952059,
133.072573721411,134.070694490763,135.068815260115,136.066936029467,137.065056798819,
138.063177568171,139.061298337523,140.059419106876,141.057539876228,142.05566064558,
143.053781414932,144.051902184284,145.050022953636,146.048143722988,147.04626449234,
148.044385261692,149.042506031044,150.040626800396,151.038747569748,152.0368683391,
153.034989108453,154.033109877805,155.031230647157,156.029351416509,157.027472185861,
158.025592955213,159.023713724565),.UNSPECIFIED.);
#1333=B_SPLINE_SURFACE_WITH_KNOTS('',3,3,((#29471,#29472,#29473,#29474,
#29475,#29476,#29477,#29478,#29479,#29480,#29481,#29482,#29483,#29484,#29485,
#29486,#29487,#29488,#29489,#29490,#29491,#29492,#29493,#29494,#29495,#29496,
#29497,#29498,#29499,#29500,#29501,#29502,#29503,#29504,#29505,#29506,#29507,
#29508,#29509,#29510,#29511,#29512,#29513,#29514,#29515,#29516,#29517,#29518,
#29519,#29520,#29521,#29522,#29523,#29524,#29525,#29526,#29527,#29528,#29529,
#29530,#29531,#29532,#29533,#29534,#29535,#29536,#29537,#29538,#29539,#29540,
#29541,#29542,#29543,#29544,#29545,#29546,#29547,#29548,#29549,#29550,#29551,
#29552,#29553,#29554,#29555,#29556,#29557,#29558,#29559,#29560,#29561,#29562,
#29563,#29564,#29565,#29566,#29567,#29568,#29569,#29570,#29571,#29572,#29573,
#29574,#29575,#29576,#29577,#29578,#29579,#29580,#29581,#29582,#29583,#29584,
#29585,#29586,#29587,#29588,#29589,#29590,#29591,#29592,#29593,#29594,#29595,
#29596,#29597,#29598,#29599,#29600,#29601,#29602,#29603,#29604,#29605,#29606,
#29607,#29608,#29609,#29610,#29611,#29612,#29613,#29614,#29615,#29616,#29617,
#29618,#29619,#29620,#29621,#29622,#29623,#29624),(#29625,#29626,#29627,
#29628,#29629,#29630,#29631,#29632,#29633,#29634,#29635,#29636,#29637,#29638,
#29639,#29640,#29641,#29642,#29643,#29644,#29645,#29646,#29647,#29648,#29649,
#29650,#29651,#29652,#29653,#29654,#29655,#29656,#29657,#29658,#29659,#29660,
#29661,#29662,#29663,#29664,#29665,#29666,#29667,#29668,#29669,#29670,#29671,
#29672,#29673,#29674,#29675,#29676,#29677,#29678,#29679,#29680,#29681,#29682,
#29683,#29684,#29685,#29686,#29687,#29688,#29689,#29690,#29691,#29692,#29693,
#29694,#29695,#29696,#29697,#29698,#29699,#29700,#29701,#29702,#29703,#29704,
#29705,#29706,#29707,#29708,#29709,#29710,#29711,#29712,#29713,#29714,#29715,
#29716,#29717,#29718,#29719,#29720,#29721,#29722,#29723,#29724,#29725,#29726,
#29727,#29728,#29729,#29730,#29731,#29732,#29733,#29734,#29735,#29736,#29737,
#29738,#29739,#29740,#29741,#29742,#29743,#29744,#29745,#29746,#29747,#29748,
#29749,#29750,#29751,#29752,#29753,#29754,#29755,#29756,#29757,#29758,#29759,
#29760,#29761,#29762,#29763,#29764,#29765,#29766,#29767,#29768,#29769,#29770,
#29771,#29772,#29773,#29774,#29775,#29776,#29777,#29778),(#29779,#29780,
#29781,#29782,#29783,#29784,#29785,#29786,#29787,#29788,#29789,#29790,#29791,
#29792,#29793,#29794,#29795,#29796,#29797,#29798,#29799,#29800,#29801,#29802,
#29803,#29804,#29805,#29806,#29807,#29808,#29809,#29810,#29811,#29812,#29813,
#29814,#29815,#29816,#29817,#29818,#29819,#29820,#29821,#29822,#29823,#29824,
#29825,#29826,#29827,#29828,#29829,#29830,#29831,#29832,#29833,#29834,#29835,
#29836,#29837,#29838,#29839,#29840,#29841,#29842,#29843,#29844,#29845,#29846,
#29847,#29848,#29849,#29850,#29851,#29852,#29853,#29854,#29855,#29856,#29857,
#29858,#29859,#29860,#29861,#29862,#29863,#29864,#29865,#29866,#29867,#29868,
#29869,#29870,#29871,#29872,#29873,#29874,#29875,#29876,#29877,#29878,#29879,
#29880,#29881,#29882,#29883,#29884,#29885,#29886,#29887,#29888,#29889,#29890,
#29891,#29892,#29893,#29894,#29895,#29896,#29897,#29898,#29899,#29900,#29901,
#29902,#29903,#29904,#29905,#29906,#29907,#29908,#29909,#29910,#29911,#29912,
#29913,#29914,#29915,#29916,#29917,#29918,#29919,#29920,#29921,#29922,#29923,
#29924,#29925,#29926,#29927,#29928,#29929,#29930,#29931,#29932),(#29933,
#29934,#29935,#29936,#29937,#29938,#29939,#29940,#29941,#29942,#29943,#29944,
#29945,#29946,#29947,#29948,#29949,#29950,#29951,#29952,#29953,#29954,#29955,
#29956,#29957,#29958,#29959,#29960,#29961,#29962,#29963,#29964,#29965,#29966,
#29967,#29968,#29969,#29970,#29971,#29972,#29973,#29974,#29975,#29976,#29977,
#29978,#29979,#29980,#29981,#29982,#29983,#29984,#29985,#29986,#29987,#29988,
#29989,#29990,#29991,#29992,#29993,#29994,#29995,#29996,#29997,#29998,#29999,
#30000,#30001,#30002,#30003,#30004,#30005,#30006,#30007,#30008,#30009,#30010,
#30011,#30012,#30013,#30014,#30015,#30016,#30017,#30018,#30019,#30020,#30021,
#30022,#30023,#30024,#30025,#30026,#30027,#30028,#30029,#30030,#30031,#30032,
#30033,#30034,#30035,#30036,#30037,#30038,#30039,#30040,#30041,#30042,#30043,
#30044,#30045,#30046,#30047,#30048,#30049,#30050,#30051,#30052,#30053,#30054,
#30055,#30056,#30057,#30058,#30059,#30060,#30061,#30062,#30063,#30064,#30065,
#30066,#30067,#30068,#30069,#30070,#30071,#30072,#30073,#30074,#30075,#30076,
#30077,#30078,#30079,#30080,#30081,#30082,#30083,#30084,#30085,#30086)),
 .UNSPECIFIED.,.F.,.F.,.F.,(4,4),(4,1,1,1,1,1,1,1,1,1,1,1,1,1,1,1,1,1,1,
1,1,1,1,1,1,1,1,1,1,1,1,1,1,1,1,1,1,1,1,1,1,1,1,1,1,1,1,1,1,1,1,1,1,1,1,
1,1,1,1,1,1,1,1,1,1,1,1,1,1,1,1,1,1,1,1,1,1,1,1,1,1,1,1,1,1,1,1,1,1,1,1,
1,1,1,1,1,1,1,1,1,1,1,1,1,1,1,1,1,1,1,1,1,1,1,1,1,1,1,1,1,1,1,1,1,1,1,1,
1,1,1,1,1,1,1,1,1,1,1,1,1,1,1,1,1,1,1,1,1,1,1,1,4),(0.,0.0658467982010769),
(11.6150328478183,12.6131536171704,13.6112743865225,14.6093951558746,15.6075159252266,
16.6056366945787,17.6037574639308,18.6018782332829,19.599999002635,20.598119771987,
21.5962405413391,22.5943613106912,23.5924820800433,24.5906028493954,25.5887236187474,
26.5868443880995,27.5849651574516,28.5830859268037,29.5812066961557,30.5793274655078,
31.5774482348599,32.575569004212,33.5736897735641,34.5718105429161,35.5699313122682,
36.5680520816203,37.5661728509724,38.5642936203245,39.5624143896765,40.5605351590286,
41.5586559283807,42.5567766977328,43.5548974670848,44.5530182364369,45.551139005789,
46.5492597751411,47.5473805444932,48.5455013138453,49.5436220831973,50.5417428525494,
51.5398636219015,52.5379843912536,53.5361051606056,54.5342259299577,55.5323466993098,
56.5304674686619,57.528588238014,58.526709007366,59.5248297767181,60.5229505460702,
61.5210713154223,62.5191920847743,63.5173128541264,64.5154336234785,65.5135543928306,
66.5116751621827,67.5097959315347,68.5079167008868,69.5060374702389,70.504158239591,
71.502279008943,72.5003997782951,73.4985205476472,74.4966413169993,75.4947620863514,
76.4928828557034,77.4910036250555,78.4891243944076,79.4872451637597,80.4853659331118,
81.4834867024638,82.4816074718159,83.479728241168,84.4778490105201,85.4759697798722,
86.4740905492242,87.4722113185763,88.4703320879284,89.4684528572805,90.4665736266326,
91.4646943959846,92.4628151653367,93.4609359346888,94.4590567040409,95.4571774733929,
96.455298242745,97.4534190120971,98.4515397814492,99.4496605508013,100.447781320153,
101.445902089505,102.444022858857,103.44214362821,104.440264397562,105.438385166914,
106.436505936266,107.434626705618,108.43274747497,109.430868244322,110.428989013674,
111.427109783026,112.425230552378,113.42335132173,114.421472091082,115.419592860435,
116.417713629787,117.415834399139,118.413955168491,119.412075937843,120.410196707195,
121.408317476547,122.406438245899,123.404559015251,124.402679784603,125.400800553955,
126.398921323307,127.397042092659,128.395162862012,129.393283631364,130.391404400716,
131.389525170068,132.38764593942,133.385766708772,134.383887478124,135.382008247476,
136.380129016828,137.37824978618,138.376370555532,139.374491324884,140.372612094236,
141.370732863589,142.368853632941,143.366974402293,144.365095171645,145.363215940997,
146.361336710349,147.359457479701,148.357578249053,149.355699018405,150.353819787757,
151.351940557109,152.350061326461,153.348182095814,154.346302865166,155.344423634518,
156.34254440387,157.340665173222,158.338785942574,159.336906711926,160.335027481278,
161.33314825063,162.331269019982),.UNSPECIFIED.);
#1334=B_SPLINE_SURFACE_WITH_KNOTS('',3,3,((#31091,#31092,#31093,#31094,
#31095),(#31096,#31097,#31098,#31099,#31100),(#31101,#31102,#31103,#31104,
#31105),(#31106,#31107,#31108,#31109,#31110)),.UNSPECIFIED.,.F.,.F.,.F.,
(4,4),(4,1,4),(0.,1.),(0.0907141004940068,0.343792306535718,0.681229914591334),
 .UNSPECIFIED.);
#1335=B_SPLINE_SURFACE_WITH_KNOTS('',3,3,((#31159,#31160,#31161,#31162,
#31163),(#31164,#31165,#31166,#31167,#31168),(#31169,#31170,#31171,#31172,
#31173),(#31174,#31175,#31176,#31177,#31178)),.UNSPECIFIED.,.F.,.F.,.F.,
(4,4),(4,1,4),(0.,1.),(0.0907141004940068,0.343792306535718,0.681229914591334),
 .UNSPECIFIED.);
#1336=B_SPLINE_SURFACE_WITH_KNOTS('',3,3,((#31219,#31220,#31221,#31222,
#31223),(#31224,#31225,#31226,#31227,#31228),(#31229,#31230,#31231,#31232,
#31233),(#31234,#31235,#31236,#31237,#31238)),.UNSPECIFIED.,.F.,.F.,.F.,
(4,4),(4,1,4),(0.,1.),(0.0907141004940071,0.343792306535719,0.681229914591334),
 .UNSPECIFIED.);
#1337=B_SPLINE_SURFACE_WITH_KNOTS('',3,3,((#31295,#31296,#31297,#31298,
#31299),(#31300,#31301,#31302,#31303,#31304),(#31305,#31306,#31307,#31308,
#31309),(#31310,#31311,#31312,#31313,#31314)),.UNSPECIFIED.,.F.,.F.,.F.,
(4,4),(4,1,4),(0.,1.),(0.0907141004940069,0.428151708549622,0.681229914591334),
 .UNSPECIFIED.);
#1338=B_SPLINE_SURFACE_WITH_KNOTS('',3,3,((#31355,#31356,#31357,#31358,
#31359),(#31360,#31361,#31362,#31363,#31364),(#31365,#31366,#31367,#31368,
#31369),(#31370,#31371,#31372,#31373,#31374)),.UNSPECIFIED.,.F.,.F.,.F.,
(4,4),(4,1,4),(0.,1.),(0.090714100494007,0.428151708549622,0.681229914591334),
 .UNSPECIFIED.);
#1339=B_SPLINE_SURFACE_WITH_KNOTS('',3,3,((#31436,#31437,#31438,#31439,
#31440),(#31441,#31442,#31443,#31444,#31445),(#31446,#31447,#31448,#31449,
#31450),(#31451,#31452,#31453,#31454,#31455)),.UNSPECIFIED.,.F.,.F.,.F.,
(4,4),(4,1,4),(0.,1.),(0.0907141004940075,0.343792306535719,0.681229914591334),
 .UNSPECIFIED.);
#1340=FACE_BOUND('',#2515,.T.);
#1341=FACE_BOUND('',#2527,.T.);
#1342=FACE_BOUND('',#2540,.T.);
#1343=FACE_BOUND('',#2556,.T.);
#1344=FACE_BOUND('',#2564,.T.);
#1345=FACE_BOUND('',#2565,.T.);
#1346=FACE_BOUND('',#2566,.T.);
#1347=FACE_BOUND('',#2567,.T.);
#1348=FACE_BOUND('',#2581,.T.);
#1349=FACE_BOUND('',#2582,.T.);
#1350=FACE_BOUND('',#2583,.T.);
#1351=FACE_BOUND('',#2584,.T.);
#1352=FACE_BOUND('',#2609,.T.);
#1353=FACE_BOUND('',#2612,.T.);
#1354=FACE_BOUND('',#2618,.T.);
#1355=FACE_BOUND('',#2621,.T.);
#1356=FACE_BOUND('',#2627,.T.);
#1357=FACE_BOUND('',#2630,.T.);
#1358=FACE_BOUND('',#2653,.T.);
#1359=FACE_BOUND('',#2660,.T.);
#1360=FACE_BOUND('',#2665,.T.);
#1361=FACE_BOUND('',#2755,.T.);
#1362=FACE_BOUND('',#2758,.T.);
#1363=FACE_BOUND('',#2759,.T.);
#1364=FACE_BOUND('',#2762,.T.);
#1365=FACE_BOUND('',#2766,.T.);
#1366=FACE_BOUND('',#2777,.T.);
#1367=FACE_BOUND('',#2778,.T.);
#1368=FACE_BOUND('',#2780,.T.);
#1369=FACE_BOUND('',#2783,.T.);
#1370=FACE_BOUND('',#2876,.T.);
#1371=FACE_BOUND('',#2878,.T.);
#1372=FACE_BOUND('',#2881,.T.);
#1373=FACE_BOUND('',#2882,.T.);
#1374=FACE_BOUND('',#2885,.T.);
#1375=FACE_BOUND('',#2887,.T.);
#1376=FACE_BOUND('',#2889,.T.);
#1377=FACE_BOUND('',#2893,.T.);
#1378=FACE_BOUND('',#2895,.T.);
#1379=FACE_BOUND('',#2899,.T.);
#1380=FACE_BOUND('',#2905,.T.);
#1381=FACE_BOUND('',#2909,.T.);
#1382=FACE_BOUND('',#2913,.T.);
#1383=FACE_BOUND('',#2917,.T.);
#1384=FACE_BOUND('',#2921,.T.);
#1385=FACE_BOUND('',#2927,.T.);
#1386=FACE_BOUND('',#2930,.T.);
#1387=FACE_BOUND('',#2935,.T.);
#1388=FACE_BOUND('',#2940,.T.);
#1389=FACE_BOUND('',#2942,.T.);
#1390=FACE_BOUND('',#2946,.T.);
#1391=FACE_BOUND('',#2949,.T.);
#1392=FACE_BOUND('',#2958,.T.);
#1393=FACE_BOUND('',#2959,.T.);
#1394=FACE_BOUND('',#2969,.T.);
#1395=FACE_BOUND('',#2970,.T.);
#1396=FACE_BOUND('',#2997,.T.);
#1397=FACE_BOUND('',#3062,.T.);
#1398=FACE_BOUND('',#3210,.T.);
#1399=FACE_BOUND('',#3215,.T.);
#1400=FACE_BOUND('',#3220,.T.);
#1401=FACE_BOUND('',#3223,.T.);
#1402=FACE_BOUND('',#3228,.T.);
#1403=FACE_BOUND('',#3261,.T.);
#1404=FACE_BOUND('',#3268,.T.);
#1405=CIRCLE('',#12617,0.8);
#1406=CIRCLE('',#12618,0.8);
#1407=CIRCLE('',#12619,1.35);
#1408=CIRCLE('',#12631,1.35);
#1409=CIRCLE('',#12644,1.35);
#1410=CIRCLE('',#12660,0.8);
#1411=CIRCLE('',#12661,0.8);
#1412=CIRCLE('',#12662,1.35);
#1413=CIRCLE('',#12668,0.39);
#1414=CIRCLE('',#12669,0.39);
#1415=CIRCLE('',#12670,0.39);
#1416=CIRCLE('',#12671,0.39);
#1417=CIRCLE('',#12680,0.39);
#1418=CIRCLE('',#12681,0.39);
#1419=CIRCLE('',#12682,0.39);
#1420=CIRCLE('',#12683,0.39);
#1421=CIRCLE('',#12691,0.33);
#1422=CIRCLE('',#12693,0.33);
#1423=CIRCLE('',#12696,0.33);
#1424=CIRCLE('',#12698,0.33);
#1425=CIRCLE('',#12701,0.33);
#1426=CIRCLE('',#12703,0.33);
#1427=CIRCLE('',#12706,0.33);
#1428=CIRCLE('',#12708,0.33);
#1429=CIRCLE('',#12711,1.35);
#1430=CIRCLE('',#12712,1.3);
#1431=CIRCLE('',#12714,1.3);
#1432=CIRCLE('',#12716,0.7);
#1433=CIRCLE('',#12718,0.7);
#1434=CIRCLE('',#12720,1.3);
#1435=CIRCLE('',#12722,1.3);
#1436=CIRCLE('',#12724,1.35);
#1437=CIRCLE('',#12726,1.3);
#1438=CIRCLE('',#12728,1.3);
#1439=CIRCLE('',#12730,0.7);
#1440=CIRCLE('',#12732,0.7);
#1441=CIRCLE('',#12734,1.3);
#1442=CIRCLE('',#12736,1.3);
#1443=CIRCLE('',#12739,1.3);
#1444=CIRCLE('',#12741,1.3);
#1445=CIRCLE('',#12743,0.7);
#1446=CIRCLE('',#12745,0.7);
#1447=CIRCLE('',#12747,1.3);
#1448=CIRCLE('',#12749,1.3);
#1449=CIRCLE('',#12759,0.4);
#1450=CIRCLE('',#12760,0.4);
#1451=CIRCLE('',#12762,0.4);
#1452=CIRCLE('',#12763,0.4);
#1453=CIRCLE('',#12766,0.4);
#1454=CIRCLE('',#12767,0.4);
#1455=CIRCLE('',#12769,0.4);
#1456=CIRCLE('',#12771,0.4);
#1457=CIRCLE('',#12778,1.35);
#1458=CIRCLE('',#12779,1.43535533905933);
#1459=CIRCLE('',#12780,1.43535533905933);
#1460=CIRCLE('',#12782,1.86384419177103);
#1461=CIRCLE('',#12783,1.86384419177103);
#1462=CIRCLE('',#12784,1.86384419177103);
#1463=CIRCLE('',#12785,1.86384419177103);
#1464=CIRCLE('',#12786,1.86384419177103);
#1465=CIRCLE('',#12787,1.86384419177103);
#1466=CIRCLE('',#12788,1.86384419177103);
#1467=CIRCLE('',#12789,1.86384419177103);
#1468=CIRCLE('',#12790,1.86384419177103);
#1469=CIRCLE('',#12791,1.86384419177103);
#1470=CIRCLE('',#12792,1.86384419177103);
#1471=CIRCLE('',#12793,1.86384419177103);
#1472=CIRCLE('',#12794,1.86384419177103);
#1473=CIRCLE('',#12795,1.86384419177103);
#1474=CIRCLE('',#12796,1.86384419177103);
#1475=CIRCLE('',#12797,1.86384419177103);
#1476=CIRCLE('',#12798,1.86384419177103);
#1477=CIRCLE('',#12799,1.86384419177103);
#1478=CIRCLE('',#12800,1.86384419177103);
#1479=CIRCLE('',#12801,1.86384419177103);
#1480=CIRCLE('',#12803,1.);
#1481=CIRCLE('',#12804,1.);
#1482=CIRCLE('',#12806,1.);
#1483=CIRCLE('',#12807,1.);
#1484=CIRCLE('',#12809,1.);
#1485=CIRCLE('',#12813,0.95);
#1486=CIRCLE('',#12815,1.2613587668218);
#1487=CIRCLE('',#12817,1.2613587668218);
#1488=CIRCLE('',#12819,1.2613587668218);
#1489=CIRCLE('',#12821,1.2613587668218);
#1490=CIRCLE('',#12823,1.2613587668218);
#1491=CIRCLE('',#12825,1.2613587668218);
#1492=CIRCLE('',#12827,1.2613587668218);
#1493=CIRCLE('',#12829,1.2613587668218);
#1494=CIRCLE('',#12831,1.2613587668218);
#1495=CIRCLE('',#12833,1.2613587668218);
#1496=CIRCLE('',#12835,1.2613587668218);
#1497=CIRCLE('',#12837,1.2613587668218);
#1498=CIRCLE('',#12839,1.2613587668218);
#1499=CIRCLE('',#12841,1.2613587668218);
#1500=CIRCLE('',#12843,1.2613587668218);
#1501=CIRCLE('',#12845,1.2613587668218);
#1502=CIRCLE('',#12847,1.2613587668218);
#1503=CIRCLE('',#12849,1.2613587668218);
#1504=CIRCLE('',#12851,1.2613587668218);
#1505=CIRCLE('',#12853,0.7);
#1506=CIRCLE('',#12854,1.2613587668218);
#1507=CIRCLE('',#12857,0.541);
#1508=CIRCLE('',#12859,0.501);
#1509=CIRCLE('',#12861,0.501);
#1510=CIRCLE('',#12863,0.541);
#1511=CIRCLE('',#12867,0.14);
#1512=CIRCLE('',#12868,0.1);
#1513=CIRCLE('',#12869,0.1);
#1514=CIRCLE('',#12871,0.1);
#1515=CIRCLE('',#12873,0.45);
#1516=CIRCLE('',#12876,0.5);
#1517=CIRCLE('',#12878,0.5);
#1518=CIRCLE('',#12881,0.5);
#1519=CIRCLE('',#12884,0.5);
#1520=CIRCLE('',#12886,0.45);
#1521=CIRCLE('',#12888,0.5);
#1522=CIRCLE('',#12890,0.5);
#1523=CIRCLE('',#12892,0.48);
#1524=CIRCLE('',#12894,0.48);
#1525=CIRCLE('',#12896,0.5);
#1526=CIRCLE('',#12898,0.5);
#1527=CIRCLE('',#12902,1.);
#1528=CIRCLE('',#12903,1.);
#1529=CIRCLE('',#12904,1.);
#1530=CIRCLE('',#12906,1.);
#1531=CIRCLE('',#12907,1.);
#1532=CIRCLE('',#12911,0.95);
#1533=CIRCLE('',#12913,1.4);
#1534=CIRCLE('',#12914,1.86384419177103);
#1535=CIRCLE('',#12915,1.86384419177103);
#1536=CIRCLE('',#12916,1.86384419177103);
#1537=CIRCLE('',#12917,1.86384419177103);
#1538=CIRCLE('',#12918,1.86384419177103);
#1539=CIRCLE('',#12919,1.86384419177103);
#1540=CIRCLE('',#12920,1.86384419177103);
#1541=CIRCLE('',#12921,1.86384419177103);
#1542=CIRCLE('',#12922,1.86384419177103);
#1543=CIRCLE('',#12923,1.86384419177103);
#1544=CIRCLE('',#12924,1.86384419177103);
#1545=CIRCLE('',#12925,1.86384419177103);
#1546=CIRCLE('',#12926,1.86384419177103);
#1547=CIRCLE('',#12927,1.86384419177103);
#1548=CIRCLE('',#12928,1.86384419177103);
#1549=CIRCLE('',#12929,1.86384419177103);
#1550=CIRCLE('',#12930,1.86384419177103);
#1551=CIRCLE('',#12931,1.86384419177103);
#1552=CIRCLE('',#12932,1.86384419177103);
#1553=CIRCLE('',#12933,1.86384419177103);
#1554=CIRCLE('',#12935,1.2613587668218);
#1555=CIRCLE('',#12937,1.2613587668218);
#1556=CIRCLE('',#12939,1.2613587668218);
#1557=CIRCLE('',#12941,1.2613587668218);
#1558=CIRCLE('',#12943,1.2613587668218);
#1559=CIRCLE('',#12945,1.2613587668218);
#1560=CIRCLE('',#12947,1.2613587668218);
#1561=CIRCLE('',#12949,1.2613587668218);
#1562=CIRCLE('',#12951,1.2613587668218);
#1563=CIRCLE('',#12953,1.2613587668218);
#1564=CIRCLE('',#12955,1.2613587668218);
#1565=CIRCLE('',#12957,1.2613587668218);
#1566=CIRCLE('',#12959,1.2613587668218);
#1567=CIRCLE('',#12961,1.2613587668218);
#1568=CIRCLE('',#12963,1.2613587668218);
#1569=CIRCLE('',#12965,1.2613587668218);
#1570=CIRCLE('',#12967,1.2613587668218);
#1571=CIRCLE('',#12969,1.2613587668218);
#1572=CIRCLE('',#12971,1.2613587668218);
#1573=CIRCLE('',#12973,0.7);
#1574=CIRCLE('',#12974,1.2613587668218);
#1575=CIRCLE('',#12978,0.541);
#1576=CIRCLE('',#12980,0.501);
#1577=CIRCLE('',#12982,0.501);
#1578=CIRCLE('',#12984,0.541);
#1579=CIRCLE('',#12988,1.06);
#1580=CIRCLE('',#12989,0.76);
#1581=CIRCLE('',#12991,1.06);
#1582=CIRCLE('',#12992,0.76);
#1583=CIRCLE('',#12995,1.06);
#1584=CIRCLE('',#12997,1.06);
#1585=CIRCLE('',#12998,0.76);
#1586=CIRCLE('',#13000,1.06);
#1587=CIRCLE('',#13001,0.76);
#1588=CIRCLE('',#13004,1.06);
#1589=CIRCLE('',#13005,1.06);
#1590=CIRCLE('',#13006,1.06);
#1591=CIRCLE('',#13007,1.06);
#1592=CIRCLE('',#13008,1.06);
#1593=CIRCLE('',#13009,1.06);
#1594=CIRCLE('',#13010,1.06);
#1595=CIRCLE('',#13011,1.06);
#1596=CIRCLE('',#13013,0.23815);
#1597=CIRCLE('',#13014,0.23815);
#1598=CIRCLE('',#13016,1.06);
#1599=CIRCLE('',#13017,1.06);
#1600=CIRCLE('',#13018,1.06);
#1601=CIRCLE('',#13019,1.06);
#1602=CIRCLE('',#13020,1.06);
#1603=CIRCLE('',#13021,1.06);
#1604=CIRCLE('',#13022,1.06);
#1605=CIRCLE('',#13023,1.06);
#1606=CIRCLE('',#13026,0.74);
#1607=CIRCLE('',#13027,0.74);
#1608=CIRCLE('',#13028,0.74);
#1609=CIRCLE('',#13029,0.74);
#1610=CIRCLE('',#13030,0.74);
#1611=CIRCLE('',#13031,0.74);
#1612=CIRCLE('',#13032,0.74);
#1613=CIRCLE('',#13033,0.74);
#1614=CIRCLE('',#13034,0.74);
#1615=CIRCLE('',#13036,0.74);
#1616=CIRCLE('',#13038,0.23815);
#1617=CIRCLE('',#13039,0.23815);
#1618=CIRCLE('',#13042,0.74);
#1619=CIRCLE('',#13044,0.23815);
#1620=CIRCLE('',#13045,0.23815);
#1621=CIRCLE('',#13048,0.74);
#1622=CIRCLE('',#13049,0.74);
#1623=CIRCLE('',#13051,0.23815);
#1624=CIRCLE('',#13052,0.23815);
#1625=CIRCLE('',#13055,0.74);
#1626=CIRCLE('',#13057,0.23815);
#1627=CIRCLE('',#13058,0.23815);
#1628=CIRCLE('',#13061,0.74);
#1629=CIRCLE('',#13063,0.23815);
#1630=CIRCLE('',#13064,0.23815);
#1631=CIRCLE('',#13066,1.06);
#1632=CIRCLE('',#13069,0.74);
#1633=CIRCLE('',#13070,0.74);
#1634=CIRCLE('',#13071,0.74);
#1635=CIRCLE('',#13074,0.23815);
#1636=CIRCLE('',#13075,0.23815);
#1637=CIRCLE('',#13078,1.27);
#1638=CIRCLE('',#13080,1.3);
#1639=CIRCLE('',#13082,1.3);
#1640=CIRCLE('',#13084,1.27);
#1641=CIRCLE('',#13088,0.5);
#1642=CIRCLE('',#13089,0.5);
#1643=CIRCLE('',#13091,0.53);
#1644=CIRCLE('',#13094,0.53);
#1645=CIRCLE('',#13098,0.5);
#1646=CIRCLE('',#13099,0.5);
#1647=CIRCLE('',#13101,0.8);
#1648=CIRCLE('',#13103,0.8);
#1649=CIRCLE('',#13115,0.48);
#1650=CIRCLE('',#13117,0.48);
#1651=CIRCLE('',#13120,0.6);
#1652=CIRCLE('',#13121,0.05);
#1653=CIRCLE('',#13122,0.05);
#1654=CIRCLE('',#13126,0.05);
#1655=CIRCLE('',#13128,0.05);
#1656=CIRCLE('',#13134,0.6);
#1657=CIRCLE('',#13138,0.1954);
#1658=CIRCLE('',#13145,0.15555);
#1659=CIRCLE('',#13147,0.15555);
#1660=CIRCLE('',#13153,0.1954);
#1661=CIRCLE('',#13154,0.1954);
#1662=CIRCLE('',#13156,0.1954);
#1663=CIRCLE('',#13157,0.1954);
#1664=CIRCLE('',#13158,0.15555);
#1665=CIRCLE('',#13168,0.17);
#1666=CIRCLE('',#13171,0.1954);
#1667=CIRCLE('',#13173,0.125);
#1668=CIRCLE('',#13177,0.2942);
#1669=CIRCLE('',#13202,0.237175);
#1670=CIRCLE('',#13204,0.237175);
#1671=CIRCLE('',#13228,0.2942);
#1672=CIRCLE('',#13229,0.2942);
#1673=CIRCLE('',#13230,0.237175);
#1674=CIRCLE('',#13233,0.249992666559108);
#1675=CIRCLE('',#13243,0.5);
#1676=CIRCLE('',#13246,0.5);
#1677=CIRCLE('',#13249,0.5);
#1678=CIRCLE('',#13252,0.5);
#1679=CIRCLE('',#13255,0.5);
#1680=CIRCLE('',#13258,0.5);
#1681=CIRCLE('',#13261,0.5);
#1682=CIRCLE('',#13264,0.5);
#1683=CIRCLE('',#13267,0.5);
#1684=CIRCLE('',#13270,0.5);
#1685=CIRCLE('',#13273,0.5);
#1686=CIRCLE('',#13276,0.5);
#1687=CIRCLE('',#13279,0.5);
#1688=CIRCLE('',#13282,0.5);
#1689=CIRCLE('',#13285,0.5);
#1690=CIRCLE('',#13288,0.5);
#1691=CIRCLE('',#13291,0.5);
#1692=CIRCLE('',#13292,0.5);
#1693=CIRCLE('',#13295,0.5);
#1694=CIRCLE('',#13296,0.5);
#1695=CIRCLE('',#13299,0.5);
#1696=CIRCLE('',#13302,0.5);
#1697=CIRCLE('',#13305,0.5);
#1698=CIRCLE('',#13308,0.5);
#1699=CIRCLE('',#13311,0.5);
#1700=CIRCLE('',#13314,0.5);
#1701=CIRCLE('',#13317,0.5);
#1702=CIRCLE('',#13320,0.5);
#1703=CIRCLE('',#13323,0.5);
#1704=CIRCLE('',#13326,0.5);
#1705=CIRCLE('',#13329,0.5);
#1706=CIRCLE('',#13332,0.5);
#1707=CIRCLE('',#13335,0.5);
#1708=CIRCLE('',#13338,0.5);
#1709=CIRCLE('',#13341,0.5);
#1710=CIRCLE('',#13344,0.5);
#1711=CIRCLE('',#13347,0.5);
#1712=CIRCLE('',#13350,0.5);
#1713=CIRCLE('',#13353,0.5);
#1714=CIRCLE('',#13356,0.5);
#1715=CIRCLE('',#13359,0.5);
#1716=CIRCLE('',#13362,0.5);
#1717=CIRCLE('',#13365,0.5);
#1718=CIRCLE('',#13368,0.5);
#1719=CIRCLE('',#13371,0.5);
#1720=CIRCLE('',#13374,0.5);
#1721=CIRCLE('',#13377,0.5);
#1722=CIRCLE('',#13380,0.5);
#1723=CIRCLE('',#13383,0.5);
#1724=CIRCLE('',#13386,0.5);
#1725=CIRCLE('',#13389,0.5);
#1726=CIRCLE('',#13392,0.5);
#1727=CIRCLE('',#13395,0.5);
#1728=CIRCLE('',#13398,0.5);
#1729=CIRCLE('',#13400,0.5);
#1730=CIRCLE('',#13404,0.5);
#1731=CIRCLE('',#13407,0.5);
#1732=CIRCLE('',#13410,0.5);
#1733=CIRCLE('',#13413,0.5);
#1734=CIRCLE('',#13416,0.5);
#1735=CIRCLE('',#13419,0.5);
#1736=CIRCLE('',#13422,0.5);
#1737=CIRCLE('',#13425,0.5);
#1738=CIRCLE('',#13428,0.5);
#1739=CIRCLE('',#13431,0.5);
#1740=CIRCLE('',#13434,0.5);
#1741=CIRCLE('',#13437,0.5);
#1742=CIRCLE('',#13440,0.5);
#1743=CIRCLE('',#13443,0.5);
#1744=CIRCLE('',#13446,0.5);
#1745=CIRCLE('',#13449,0.5);
#1746=CIRCLE('',#13452,0.5);
#1747=CIRCLE('',#13455,0.5);
#1748=CIRCLE('',#13458,0.5);
#1749=CIRCLE('',#13460,0.298);
#1750=CIRCLE('',#13461,0.025);
#1751=CIRCLE('',#13462,0.323);
#1752=CIRCLE('',#13464,0.298);
#1753=CIRCLE('',#13466,0.48);
#1754=CIRCLE('',#13468,0.26);
#1755=CIRCLE('',#13471,0.2942);
#1756=CIRCLE('',#13474,0.5);
#1757=CIRCLE('',#13476,0.5);
#1758=CIRCLE('',#13477,0.5);
#1759=CIRCLE('',#13478,0.5);
#1760=CIRCLE('',#13479,0.5);
#1761=CIRCLE('',#13480,0.5);
#1762=CIRCLE('',#13481,0.5);
#1763=CIRCLE('',#13482,0.5);
#1764=CIRCLE('',#13483,0.5);
#1765=CIRCLE('',#13484,0.5);
#1766=CIRCLE('',#13485,0.5);
#1767=CIRCLE('',#13486,0.5);
#1768=CIRCLE('',#13487,0.5);
#1769=CIRCLE('',#13488,0.5);
#1770=CIRCLE('',#13489,0.5);
#1771=CIRCLE('',#13490,0.5);
#1772=CIRCLE('',#13491,0.5);
#1773=CIRCLE('',#13492,0.5);
#1774=CIRCLE('',#13493,0.5);
#1775=CIRCLE('',#13494,0.5);
#1776=CIRCLE('',#13495,0.5);
#1777=CIRCLE('',#13496,0.5);
#1778=CIRCLE('',#13497,0.5);
#1779=CIRCLE('',#13498,0.5);
#1780=CIRCLE('',#13499,0.5);
#1781=CIRCLE('',#13500,0.5);
#1782=CIRCLE('',#13501,0.5);
#1783=CIRCLE('',#13502,0.5);
#1784=CIRCLE('',#13503,0.5);
#1785=CIRCLE('',#13504,0.5);
#1786=CIRCLE('',#13505,0.5);
#1787=CIRCLE('',#13506,0.5);
#1788=CIRCLE('',#13507,0.5);
#1789=CIRCLE('',#13508,0.5);
#1790=CIRCLE('',#13509,0.5);
#1791=CIRCLE('',#13510,0.5);
#1792=CIRCLE('',#13511,0.5);
#1793=CIRCLE('',#13513,0.46);
#1794=CIRCLE('',#13517,0.58);
#1795=CIRCLE('',#13518,0.6);
#1796=CIRCLE('',#13519,0.6);
#1797=CIRCLE('',#13521,0.34);
#1798=CIRCLE('',#13523,0.6);
#1799=CIRCLE('',#13525,0.34);
#1800=CIRCLE('',#13526,0.32);
#1801=CIRCLE('',#13527,0.32);
#1802=CIRCLE('',#13529,0.32);
#1803=CIRCLE('',#13530,0.32);
#1804=CIRCLE('',#13532,0.58);
#1805=CIRCLE('',#13552,0.475);
#1806=CIRCLE('',#13554,0.493186533479473);
#1807=CIRCLE('',#13556,0.493186533479473);
#1808=CIRCLE('',#13558,0.493186533479473);
#1809=CIRCLE('',#13560,0.493186533479473);
#1810=CIRCLE('',#13562,0.493186533479473);
#1811=CIRCLE('',#13564,0.493186533479473);
#1812=CIRCLE('',#13566,0.454);
#1813=CIRCLE('',#13568,0.366);
#1814=CIRCLE('',#13570,0.330150757595083);
#1815=CIRCLE('',#13572,0.319849242404917);
#1816=CIRCLE('',#13574,0.305);
#1817=CIRCLE('',#13576,0.305);
#1818=CIRCLE('',#13578,0.345);
#1819=FACE_OUTER_BOUND('',#2513,.T.);
#1820=FACE_OUTER_BOUND('',#2514,.T.);
#1821=FACE_OUTER_BOUND('',#2516,.T.);
#1822=FACE_OUTER_BOUND('',#2517,.T.);
#1823=FACE_OUTER_BOUND('',#2518,.T.);
#1824=FACE_OUTER_BOUND('',#2519,.T.);
#1825=FACE_OUTER_BOUND('',#2520,.T.);
#1826=FACE_OUTER_BOUND('',#2521,.T.);
#1827=FACE_OUTER_BOUND('',#2522,.T.);
#1828=FACE_OUTER_BOUND('',#2523,.T.);
#1829=FACE_OUTER_BOUND('',#2524,.T.);
#1830=FACE_OUTER_BOUND('',#2525,.T.);
#1831=FACE_OUTER_BOUND('',#2526,.T.);
#1832=FACE_OUTER_BOUND('',#2528,.T.);
#1833=FACE_OUTER_BOUND('',#2529,.T.);
#1834=FACE_OUTER_BOUND('',#2530,.T.);
#1835=FACE_OUTER_BOUND('',#2531,.T.);
#1836=FACE_OUTER_BOUND('',#2532,.T.);
#1837=FACE_OUTER_BOUND('',#2533,.T.);
#1838=FACE_OUTER_BOUND('',#2534,.T.);
#1839=FACE_OUTER_BOUND('',#2535,.T.);
#1840=FACE_OUTER_BOUND('',#2536,.T.);
#1841=FACE_OUTER_BOUND('',#2537,.T.);
#1842=FACE_OUTER_BOUND('',#2538,.T.);
#1843=FACE_OUTER_BOUND('',#2539,.T.);
#1844=FACE_OUTER_BOUND('',#2541,.T.);
#1845=FACE_OUTER_BOUND('',#2542,.T.);
#1846=FACE_OUTER_BOUND('',#2543,.T.);
#1847=FACE_OUTER_BOUND('',#2544,.T.);
#1848=FACE_OUTER_BOUND('',#2545,.T.);
#1849=FACE_OUTER_BOUND('',#2546,.T.);
#1850=FACE_OUTER_BOUND('',#2547,.T.);
#1851=FACE_OUTER_BOUND('',#2548,.T.);
#1852=FACE_OUTER_BOUND('',#2549,.T.);
#1853=FACE_OUTER_BOUND('',#2550,.T.);
#1854=FACE_OUTER_BOUND('',#2551,.T.);
#1855=FACE_OUTER_BOUND('',#2552,.T.);
#1856=FACE_OUTER_BOUND('',#2553,.T.);
#1857=FACE_OUTER_BOUND('',#2554,.T.);
#1858=FACE_OUTER_BOUND('',#2555,.T.);
#1859=FACE_OUTER_BOUND('',#2557,.T.);
#1860=FACE_OUTER_BOUND('',#2558,.T.);
#1861=FACE_OUTER_BOUND('',#2559,.T.);
#1862=FACE_OUTER_BOUND('',#2560,.T.);
#1863=FACE_OUTER_BOUND('',#2561,.T.);
#1864=FACE_OUTER_BOUND('',#2562,.T.);
#1865=FACE_OUTER_BOUND('',#2563,.T.);
#1866=FACE_OUTER_BOUND('',#2568,.T.);
#1867=FACE_OUTER_BOUND('',#2569,.T.);
#1868=FACE_OUTER_BOUND('',#2570,.T.);
#1869=FACE_OUTER_BOUND('',#2571,.T.);
#1870=FACE_OUTER_BOUND('',#2572,.T.);
#1871=FACE_OUTER_BOUND('',#2573,.T.);
#1872=FACE_OUTER_BOUND('',#2574,.T.);
#1873=FACE_OUTER_BOUND('',#2575,.T.);
#1874=FACE_OUTER_BOUND('',#2576,.T.);
#1875=FACE_OUTER_BOUND('',#2577,.T.);
#1876=FACE_OUTER_BOUND('',#2578,.T.);
#1877=FACE_OUTER_BOUND('',#2579,.T.);
#1878=FACE_OUTER_BOUND('',#2580,.T.);
#1879=FACE_OUTER_BOUND('',#2585,.T.);
#1880=FACE_OUTER_BOUND('',#2586,.T.);
#1881=FACE_OUTER_BOUND('',#2587,.T.);
#1882=FACE_OUTER_BOUND('',#2588,.T.);
#1883=FACE_OUTER_BOUND('',#2589,.T.);
#1884=FACE_OUTER_BOUND('',#2590,.T.);
#1885=FACE_OUTER_BOUND('',#2591,.T.);
#1886=FACE_OUTER_BOUND('',#2592,.T.);
#1887=FACE_OUTER_BOUND('',#2593,.T.);
#1888=FACE_OUTER_BOUND('',#2594,.T.);
#1889=FACE_OUTER_BOUND('',#2595,.T.);
#1890=FACE_OUTER_BOUND('',#2596,.T.);
#1891=FACE_OUTER_BOUND('',#2597,.T.);
#1892=FACE_OUTER_BOUND('',#2598,.T.);
#1893=FACE_OUTER_BOUND('',#2599,.T.);
#1894=FACE_OUTER_BOUND('',#2600,.T.);
#1895=FACE_OUTER_BOUND('',#2601,.T.);
#1896=FACE_OUTER_BOUND('',#2602,.T.);
#1897=FACE_OUTER_BOUND('',#2603,.T.);
#1898=FACE_OUTER_BOUND('',#2604,.T.);
#1899=FACE_OUTER_BOUND('',#2605,.T.);
#1900=FACE_OUTER_BOUND('',#2606,.T.);
#1901=FACE_OUTER_BOUND('',#2607,.T.);
#1902=FACE_OUTER_BOUND('',#2608,.T.);
#1903=FACE_OUTER_BOUND('',#2610,.T.);
#1904=FACE_OUTER_BOUND('',#2611,.T.);
#1905=FACE_OUTER_BOUND('',#2613,.T.);
#1906=FACE_OUTER_BOUND('',#2614,.T.);
#1907=FACE_OUTER_BOUND('',#2615,.T.);
#1908=FACE_OUTER_BOUND('',#2616,.T.);
#1909=FACE_OUTER_BOUND('',#2617,.T.);
#1910=FACE_OUTER_BOUND('',#2619,.T.);
#1911=FACE_OUTER_BOUND('',#2620,.T.);
#1912=FACE_OUTER_BOUND('',#2622,.T.);
#1913=FACE_OUTER_BOUND('',#2623,.T.);
#1914=FACE_OUTER_BOUND('',#2624,.T.);
#1915=FACE_OUTER_BOUND('',#2625,.T.);
#1916=FACE_OUTER_BOUND('',#2626,.T.);
#1917=FACE_OUTER_BOUND('',#2628,.T.);
#1918=FACE_OUTER_BOUND('',#2629,.T.);
#1919=FACE_OUTER_BOUND('',#2631,.T.);
#1920=FACE_OUTER_BOUND('',#2632,.T.);
#1921=FACE_OUTER_BOUND('',#2633,.T.);
#1922=FACE_OUTER_BOUND('',#2634,.T.);
#1923=FACE_OUTER_BOUND('',#2635,.T.);
#1924=FACE_OUTER_BOUND('',#2636,.T.);
#1925=FACE_OUTER_BOUND('',#2637,.T.);
#1926=FACE_OUTER_BOUND('',#2638,.T.);
#1927=FACE_OUTER_BOUND('',#2639,.T.);
#1928=FACE_OUTER_BOUND('',#2640,.T.);
#1929=FACE_OUTER_BOUND('',#2641,.T.);
#1930=FACE_OUTER_BOUND('',#2642,.T.);
#1931=FACE_OUTER_BOUND('',#2643,.T.);
#1932=FACE_OUTER_BOUND('',#2644,.T.);
#1933=FACE_OUTER_BOUND('',#2645,.T.);
#1934=FACE_OUTER_BOUND('',#2646,.T.);
#1935=FACE_OUTER_BOUND('',#2647,.T.);
#1936=FACE_OUTER_BOUND('',#2648,.T.);
#1937=FACE_OUTER_BOUND('',#2649,.T.);
#1938=FACE_OUTER_BOUND('',#2650,.T.);
#1939=FACE_OUTER_BOUND('',#2651,.T.);
#1940=FACE_OUTER_BOUND('',#2652,.T.);
#1941=FACE_OUTER_BOUND('',#2654,.T.);
#1942=FACE_OUTER_BOUND('',#2655,.T.);
#1943=FACE_OUTER_BOUND('',#2656,.T.);
#1944=FACE_OUTER_BOUND('',#2657,.T.);
#1945=FACE_OUTER_BOUND('',#2658,.T.);
#1946=FACE_OUTER_BOUND('',#2659,.T.);
#1947=FACE_OUTER_BOUND('',#2661,.T.);
#1948=FACE_OUTER_BOUND('',#2662,.T.);
#1949=FACE_OUTER_BOUND('',#2663,.T.);
#1950=FACE_OUTER_BOUND('',#2664,.T.);
#1951=FACE_OUTER_BOUND('',#2666,.T.);
#1952=FACE_OUTER_BOUND('',#2667,.T.);
#1953=FACE_OUTER_BOUND('',#2668,.T.);
#1954=FACE_OUTER_BOUND('',#2669,.T.);
#1955=FACE_OUTER_BOUND('',#2670,.T.);
#1956=FACE_OUTER_BOUND('',#2671,.T.);
#1957=FACE_OUTER_BOUND('',#2672,.T.);
#1958=FACE_OUTER_BOUND('',#2673,.T.);
#1959=FACE_OUTER_BOUND('',#2674,.T.);
#1960=FACE_OUTER_BOUND('',#2675,.T.);
#1961=FACE_OUTER_BOUND('',#2676,.T.);
#1962=FACE_OUTER_BOUND('',#2677,.T.);
#1963=FACE_OUTER_BOUND('',#2678,.T.);
#1964=FACE_OUTER_BOUND('',#2679,.T.);
#1965=FACE_OUTER_BOUND('',#2680,.T.);
#1966=FACE_OUTER_BOUND('',#2681,.T.);
#1967=FACE_OUTER_BOUND('',#2682,.T.);
#1968=FACE_OUTER_BOUND('',#2683,.T.);
#1969=FACE_OUTER_BOUND('',#2684,.T.);
#1970=FACE_OUTER_BOUND('',#2685,.T.);
#1971=FACE_OUTER_BOUND('',#2686,.T.);
#1972=FACE_OUTER_BOUND('',#2687,.T.);
#1973=FACE_OUTER_BOUND('',#2688,.T.);
#1974=FACE_OUTER_BOUND('',#2689,.T.);
#1975=FACE_OUTER_BOUND('',#2690,.T.);
#1976=FACE_OUTER_BOUND('',#2691,.T.);
#1977=FACE_OUTER_BOUND('',#2692,.T.);
#1978=FACE_OUTER_BOUND('',#2693,.T.);
#1979=FACE_OUTER_BOUND('',#2694,.T.);
#1980=FACE_OUTER_BOUND('',#2695,.T.);
#1981=FACE_OUTER_BOUND('',#2696,.T.);
#1982=FACE_OUTER_BOUND('',#2697,.T.);
#1983=FACE_OUTER_BOUND('',#2698,.T.);
#1984=FACE_OUTER_BOUND('',#2699,.T.);
#1985=FACE_OUTER_BOUND('',#2700,.T.);
#1986=FACE_OUTER_BOUND('',#2701,.T.);
#1987=FACE_OUTER_BOUND('',#2702,.T.);
#1988=FACE_OUTER_BOUND('',#2703,.T.);
#1989=FACE_OUTER_BOUND('',#2704,.T.);
#1990=FACE_OUTER_BOUND('',#2705,.T.);
#1991=FACE_OUTER_BOUND('',#2706,.T.);
#1992=FACE_OUTER_BOUND('',#2707,.T.);
#1993=FACE_OUTER_BOUND('',#2708,.T.);
#1994=FACE_OUTER_BOUND('',#2709,.T.);
#1995=FACE_OUTER_BOUND('',#2710,.T.);
#1996=FACE_OUTER_BOUND('',#2711,.T.);
#1997=FACE_OUTER_BOUND('',#2712,.T.);
#1998=FACE_OUTER_BOUND('',#2713,.T.);
#1999=FACE_OUTER_BOUND('',#2714,.T.);
#2000=FACE_OUTER_BOUND('',#2715,.T.);
#2001=FACE_OUTER_BOUND('',#2716,.T.);
#2002=FACE_OUTER_BOUND('',#2717,.T.);
#2003=FACE_OUTER_BOUND('',#2718,.T.);
#2004=FACE_OUTER_BOUND('',#2719,.T.);
#2005=FACE_OUTER_BOUND('',#2720,.T.);
#2006=FACE_OUTER_BOUND('',#2721,.T.);
#2007=FACE_OUTER_BOUND('',#2722,.T.);
#2008=FACE_OUTER_BOUND('',#2723,.T.);
#2009=FACE_OUTER_BOUND('',#2724,.T.);
#2010=FACE_OUTER_BOUND('',#2725,.T.);
#2011=FACE_OUTER_BOUND('',#2726,.T.);
#2012=FACE_OUTER_BOUND('',#2727,.T.);
#2013=FACE_OUTER_BOUND('',#2728,.T.);
#2014=FACE_OUTER_BOUND('',#2729,.T.);
#2015=FACE_OUTER_BOUND('',#2730,.T.);
#2016=FACE_OUTER_BOUND('',#2731,.T.);
#2017=FACE_OUTER_BOUND('',#2732,.T.);
#2018=FACE_OUTER_BOUND('',#2733,.T.);
#2019=FACE_OUTER_BOUND('',#2734,.T.);
#2020=FACE_OUTER_BOUND('',#2735,.T.);
#2021=FACE_OUTER_BOUND('',#2736,.T.);
#2022=FACE_OUTER_BOUND('',#2737,.T.);
#2023=FACE_OUTER_BOUND('',#2738,.T.);
#2024=FACE_OUTER_BOUND('',#2739,.T.);
#2025=FACE_OUTER_BOUND('',#2740,.T.);
#2026=FACE_OUTER_BOUND('',#2741,.T.);
#2027=FACE_OUTER_BOUND('',#2742,.T.);
#2028=FACE_OUTER_BOUND('',#2743,.T.);
#2029=FACE_OUTER_BOUND('',#2744,.T.);
#2030=FACE_OUTER_BOUND('',#2745,.T.);
#2031=FACE_OUTER_BOUND('',#2746,.T.);
#2032=FACE_OUTER_BOUND('',#2747,.T.);
#2033=FACE_OUTER_BOUND('',#2748,.T.);
#2034=FACE_OUTER_BOUND('',#2749,.T.);
#2035=FACE_OUTER_BOUND('',#2750,.T.);
#2036=FACE_OUTER_BOUND('',#2751,.T.);
#2037=FACE_OUTER_BOUND('',#2752,.T.);
#2038=FACE_OUTER_BOUND('',#2753,.T.);
#2039=FACE_OUTER_BOUND('',#2754,.T.);
#2040=FACE_OUTER_BOUND('',#2756,.T.);
#2041=FACE_OUTER_BOUND('',#2757,.T.);
#2042=FACE_OUTER_BOUND('',#2760,.T.);
#2043=FACE_OUTER_BOUND('',#2761,.T.);
#2044=FACE_OUTER_BOUND('',#2763,.T.);
#2045=FACE_OUTER_BOUND('',#2764,.T.);
#2046=FACE_OUTER_BOUND('',#2765,.T.);
#2047=FACE_OUTER_BOUND('',#2767,.T.);
#2048=FACE_OUTER_BOUND('',#2768,.T.);
#2049=FACE_OUTER_BOUND('',#2769,.T.);
#2050=FACE_OUTER_BOUND('',#2770,.T.);
#2051=FACE_OUTER_BOUND('',#2771,.T.);
#2052=FACE_OUTER_BOUND('',#2772,.T.);
#2053=FACE_OUTER_BOUND('',#2773,.T.);
#2054=FACE_OUTER_BOUND('',#2774,.T.);
#2055=FACE_OUTER_BOUND('',#2775,.T.);
#2056=FACE_OUTER_BOUND('',#2776,.T.);
#2057=FACE_OUTER_BOUND('',#2779,.T.);
#2058=FACE_OUTER_BOUND('',#2781,.T.);
#2059=FACE_OUTER_BOUND('',#2782,.T.);
#2060=FACE_OUTER_BOUND('',#2784,.T.);
#2061=FACE_OUTER_BOUND('',#2785,.T.);
#2062=FACE_OUTER_BOUND('',#2786,.T.);
#2063=FACE_OUTER_BOUND('',#2787,.T.);
#2064=FACE_OUTER_BOUND('',#2788,.T.);
#2065=FACE_OUTER_BOUND('',#2789,.T.);
#2066=FACE_OUTER_BOUND('',#2790,.T.);
#2067=FACE_OUTER_BOUND('',#2791,.T.);
#2068=FACE_OUTER_BOUND('',#2792,.T.);
#2069=FACE_OUTER_BOUND('',#2793,.T.);
#2070=FACE_OUTER_BOUND('',#2794,.T.);
#2071=FACE_OUTER_BOUND('',#2795,.T.);
#2072=FACE_OUTER_BOUND('',#2796,.T.);
#2073=FACE_OUTER_BOUND('',#2797,.T.);
#2074=FACE_OUTER_BOUND('',#2798,.T.);
#2075=FACE_OUTER_BOUND('',#2799,.T.);
#2076=FACE_OUTER_BOUND('',#2800,.T.);
#2077=FACE_OUTER_BOUND('',#2801,.T.);
#2078=FACE_OUTER_BOUND('',#2802,.T.);
#2079=FACE_OUTER_BOUND('',#2803,.T.);
#2080=FACE_OUTER_BOUND('',#2804,.T.);
#2081=FACE_OUTER_BOUND('',#2805,.T.);
#2082=FACE_OUTER_BOUND('',#2806,.T.);
#2083=FACE_OUTER_BOUND('',#2807,.T.);
#2084=FACE_OUTER_BOUND('',#2808,.T.);
#2085=FACE_OUTER_BOUND('',#2809,.T.);
#2086=FACE_OUTER_BOUND('',#2810,.T.);
#2087=FACE_OUTER_BOUND('',#2811,.T.);
#2088=FACE_OUTER_BOUND('',#2812,.T.);
#2089=FACE_OUTER_BOUND('',#2813,.T.);
#2090=FACE_OUTER_BOUND('',#2814,.T.);
#2091=FACE_OUTER_BOUND('',#2815,.T.);
#2092=FACE_OUTER_BOUND('',#2816,.T.);
#2093=FACE_OUTER_BOUND('',#2817,.T.);
#2094=FACE_OUTER_BOUND('',#2818,.T.);
#2095=FACE_OUTER_BOUND('',#2819,.T.);
#2096=FACE_OUTER_BOUND('',#2820,.T.);
#2097=FACE_OUTER_BOUND('',#2821,.T.);
#2098=FACE_OUTER_BOUND('',#2822,.T.);
#2099=FACE_OUTER_BOUND('',#2823,.T.);
#2100=FACE_OUTER_BOUND('',#2824,.T.);
#2101=FACE_OUTER_BOUND('',#2825,.T.);
#2102=FACE_OUTER_BOUND('',#2826,.T.);
#2103=FACE_OUTER_BOUND('',#2827,.T.);
#2104=FACE_OUTER_BOUND('',#2828,.T.);
#2105=FACE_OUTER_BOUND('',#2829,.T.);
#2106=FACE_OUTER_BOUND('',#2830,.T.);
#2107=FACE_OUTER_BOUND('',#2831,.T.);
#2108=FACE_OUTER_BOUND('',#2832,.T.);
#2109=FACE_OUTER_BOUND('',#2833,.T.);
#2110=FACE_OUTER_BOUND('',#2834,.T.);
#2111=FACE_OUTER_BOUND('',#2835,.T.);
#2112=FACE_OUTER_BOUND('',#2836,.T.);
#2113=FACE_OUTER_BOUND('',#2837,.T.);
#2114=FACE_OUTER_BOUND('',#2838,.T.);
#2115=FACE_OUTER_BOUND('',#2839,.T.);
#2116=FACE_OUTER_BOUND('',#2840,.T.);
#2117=FACE_OUTER_BOUND('',#2841,.T.);
#2118=FACE_OUTER_BOUND('',#2842,.T.);
#2119=FACE_OUTER_BOUND('',#2843,.T.);
#2120=FACE_OUTER_BOUND('',#2844,.T.);
#2121=FACE_OUTER_BOUND('',#2845,.T.);
#2122=FACE_OUTER_BOUND('',#2846,.T.);
#2123=FACE_OUTER_BOUND('',#2847,.T.);
#2124=FACE_OUTER_BOUND('',#2848,.T.);
#2125=FACE_OUTER_BOUND('',#2849,.T.);
#2126=FACE_OUTER_BOUND('',#2850,.T.);
#2127=FACE_OUTER_BOUND('',#2851,.T.);
#2128=FACE_OUTER_BOUND('',#2852,.T.);
#2129=FACE_OUTER_BOUND('',#2853,.T.);
#2130=FACE_OUTER_BOUND('',#2854,.T.);
#2131=FACE_OUTER_BOUND('',#2855,.T.);
#2132=FACE_OUTER_BOUND('',#2856,.T.);
#2133=FACE_OUTER_BOUND('',#2857,.T.);
#2134=FACE_OUTER_BOUND('',#2858,.T.);
#2135=FACE_OUTER_BOUND('',#2859,.T.);
#2136=FACE_OUTER_BOUND('',#2860,.T.);
#2137=FACE_OUTER_BOUND('',#2861,.T.);
#2138=FACE_OUTER_BOUND('',#2862,.T.);
#2139=FACE_OUTER_BOUND('',#2863,.T.);
#2140=FACE_OUTER_BOUND('',#2864,.T.);
#2141=FACE_OUTER_BOUND('',#2865,.T.);
#2142=FACE_OUTER_BOUND('',#2866,.T.);
#2143=FACE_OUTER_BOUND('',#2867,.T.);
#2144=FACE_OUTER_BOUND('',#2868,.T.);
#2145=FACE_OUTER_BOUND('',#2869,.T.);
#2146=FACE_OUTER_BOUND('',#2870,.T.);
#2147=FACE_OUTER_BOUND('',#2871,.T.);
#2148=FACE_OUTER_BOUND('',#2872,.T.);
#2149=FACE_OUTER_BOUND('',#2873,.T.);
#2150=FACE_OUTER_BOUND('',#2874,.T.);
#2151=FACE_OUTER_BOUND('',#2875,.T.);
#2152=FACE_OUTER_BOUND('',#2877,.T.);
#2153=FACE_OUTER_BOUND('',#2879,.T.);
#2154=FACE_OUTER_BOUND('',#2880,.T.);
#2155=FACE_OUTER_BOUND('',#2883,.T.);
#2156=FACE_OUTER_BOUND('',#2884,.T.);
#2157=FACE_OUTER_BOUND('',#2886,.T.);
#2158=FACE_OUTER_BOUND('',#2888,.T.);
#2159=FACE_OUTER_BOUND('',#2890,.T.);
#2160=FACE_OUTER_BOUND('',#2891,.T.);
#2161=FACE_OUTER_BOUND('',#2892,.T.);
#2162=FACE_OUTER_BOUND('',#2894,.T.);
#2163=FACE_OUTER_BOUND('',#2896,.T.);
#2164=FACE_OUTER_BOUND('',#2897,.T.);
#2165=FACE_OUTER_BOUND('',#2898,.T.);
#2166=FACE_OUTER_BOUND('',#2900,.T.);
#2167=FACE_OUTER_BOUND('',#2901,.T.);
#2168=FACE_OUTER_BOUND('',#2902,.T.);
#2169=FACE_OUTER_BOUND('',#2903,.T.);
#2170=FACE_OUTER_BOUND('',#2904,.T.);
#2171=FACE_OUTER_BOUND('',#2906,.T.);
#2172=FACE_OUTER_BOUND('',#2907,.T.);
#2173=FACE_OUTER_BOUND('',#2908,.T.);
#2174=FACE_OUTER_BOUND('',#2910,.T.);
#2175=FACE_OUTER_BOUND('',#2911,.T.);
#2176=FACE_OUTER_BOUND('',#2912,.T.);
#2177=FACE_OUTER_BOUND('',#2914,.T.);
#2178=FACE_OUTER_BOUND('',#2915,.T.);
#2179=FACE_OUTER_BOUND('',#2916,.T.);
#2180=FACE_OUTER_BOUND('',#2918,.T.);
#2181=FACE_OUTER_BOUND('',#2919,.T.);
#2182=FACE_OUTER_BOUND('',#2920,.T.);
#2183=FACE_OUTER_BOUND('',#2922,.T.);
#2184=FACE_OUTER_BOUND('',#2923,.T.);
#2185=FACE_OUTER_BOUND('',#2924,.T.);
#2186=FACE_OUTER_BOUND('',#2925,.T.);
#2187=FACE_OUTER_BOUND('',#2926,.T.);
#2188=FACE_OUTER_BOUND('',#2928,.T.);
#2189=FACE_OUTER_BOUND('',#2929,.T.);
#2190=FACE_OUTER_BOUND('',#2931,.T.);
#2191=FACE_OUTER_BOUND('',#2932,.T.);
#2192=FACE_OUTER_BOUND('',#2933,.T.);
#2193=FACE_OUTER_BOUND('',#2934,.T.);
#2194=FACE_OUTER_BOUND('',#2936,.T.);
#2195=FACE_OUTER_BOUND('',#2937,.T.);
#2196=FACE_OUTER_BOUND('',#2938,.T.);
#2197=FACE_OUTER_BOUND('',#2939,.T.);
#2198=FACE_OUTER_BOUND('',#2941,.T.);
#2199=FACE_OUTER_BOUND('',#2943,.T.);
#2200=FACE_OUTER_BOUND('',#2944,.T.);
#2201=FACE_OUTER_BOUND('',#2945,.T.);
#2202=FACE_OUTER_BOUND('',#2947,.T.);
#2203=FACE_OUTER_BOUND('',#2948,.T.);
#2204=FACE_OUTER_BOUND('',#2950,.T.);
#2205=FACE_OUTER_BOUND('',#2951,.T.);
#2206=FACE_OUTER_BOUND('',#2952,.T.);
#2207=FACE_OUTER_BOUND('',#2953,.T.);
#2208=FACE_OUTER_BOUND('',#2954,.T.);
#2209=FACE_OUTER_BOUND('',#2955,.T.);
#2210=FACE_OUTER_BOUND('',#2956,.T.);
#2211=FACE_OUTER_BOUND('',#2957,.T.);
#2212=FACE_OUTER_BOUND('',#2960,.T.);
#2213=FACE_OUTER_BOUND('',#2961,.T.);
#2214=FACE_OUTER_BOUND('',#2962,.T.);
#2215=FACE_OUTER_BOUND('',#2963,.T.);
#2216=FACE_OUTER_BOUND('',#2964,.T.);
#2217=FACE_OUTER_BOUND('',#2965,.T.);
#2218=FACE_OUTER_BOUND('',#2966,.T.);
#2219=FACE_OUTER_BOUND('',#2967,.T.);
#2220=FACE_OUTER_BOUND('',#2968,.T.);
#2221=FACE_OUTER_BOUND('',#2971,.T.);
#2222=FACE_OUTER_BOUND('',#2972,.T.);
#2223=FACE_OUTER_BOUND('',#2973,.T.);
#2224=FACE_OUTER_BOUND('',#2974,.T.);
#2225=FACE_OUTER_BOUND('',#2975,.T.);
#2226=FACE_OUTER_BOUND('',#2976,.T.);
#2227=FACE_OUTER_BOUND('',#2977,.T.);
#2228=FACE_OUTER_BOUND('',#2978,.T.);
#2229=FACE_OUTER_BOUND('',#2979,.T.);
#2230=FACE_OUTER_BOUND('',#2980,.T.);
#2231=FACE_OUTER_BOUND('',#2981,.T.);
#2232=FACE_OUTER_BOUND('',#2982,.T.);
#2233=FACE_OUTER_BOUND('',#2983,.T.);
#2234=FACE_OUTER_BOUND('',#2984,.T.);
#2235=FACE_OUTER_BOUND('',#2985,.T.);
#2236=FACE_OUTER_BOUND('',#2986,.T.);
#2237=FACE_OUTER_BOUND('',#2987,.T.);
#2238=FACE_OUTER_BOUND('',#2988,.T.);
#2239=FACE_OUTER_BOUND('',#2989,.T.);
#2240=FACE_OUTER_BOUND('',#2990,.T.);
#2241=FACE_OUTER_BOUND('',#2991,.T.);
#2242=FACE_OUTER_BOUND('',#2992,.T.);
#2243=FACE_OUTER_BOUND('',#2993,.T.);
#2244=FACE_OUTER_BOUND('',#2994,.T.);
#2245=FACE_OUTER_BOUND('',#2995,.T.);
#2246=FACE_OUTER_BOUND('',#2996,.T.);
#2247=FACE_OUTER_BOUND('',#2998,.T.);
#2248=FACE_OUTER_BOUND('',#2999,.T.);
#2249=FACE_OUTER_BOUND('',#3000,.T.);
#2250=FACE_OUTER_BOUND('',#3001,.T.);
#2251=FACE_OUTER_BOUND('',#3002,.T.);
#2252=FACE_OUTER_BOUND('',#3003,.T.);
#2253=FACE_OUTER_BOUND('',#3004,.T.);
#2254=FACE_OUTER_BOUND('',#3005,.T.);
#2255=FACE_OUTER_BOUND('',#3006,.T.);
#2256=FACE_OUTER_BOUND('',#3007,.T.);
#2257=FACE_OUTER_BOUND('',#3008,.T.);
#2258=FACE_OUTER_BOUND('',#3009,.T.);
#2259=FACE_OUTER_BOUND('',#3010,.T.);
#2260=FACE_OUTER_BOUND('',#3011,.T.);
#2261=FACE_OUTER_BOUND('',#3012,.T.);
#2262=FACE_OUTER_BOUND('',#3013,.T.);
#2263=FACE_OUTER_BOUND('',#3014,.T.);
#2264=FACE_OUTER_BOUND('',#3015,.T.);
#2265=FACE_OUTER_BOUND('',#3016,.T.);
#2266=FACE_OUTER_BOUND('',#3017,.T.);
#2267=FACE_OUTER_BOUND('',#3018,.T.);
#2268=FACE_OUTER_BOUND('',#3019,.T.);
#2269=FACE_OUTER_BOUND('',#3020,.T.);
#2270=FACE_OUTER_BOUND('',#3021,.T.);
#2271=FACE_OUTER_BOUND('',#3022,.T.);
#2272=FACE_OUTER_BOUND('',#3023,.T.);
#2273=FACE_OUTER_BOUND('',#3024,.T.);
#2274=FACE_OUTER_BOUND('',#3025,.T.);
#2275=FACE_OUTER_BOUND('',#3026,.T.);
#2276=FACE_OUTER_BOUND('',#3027,.T.);
#2277=FACE_OUTER_BOUND('',#3028,.T.);
#2278=FACE_OUTER_BOUND('',#3029,.T.);
#2279=FACE_OUTER_BOUND('',#3030,.T.);
#2280=FACE_OUTER_BOUND('',#3031,.T.);
#2281=FACE_OUTER_BOUND('',#3032,.T.);
#2282=FACE_OUTER_BOUND('',#3033,.T.);
#2283=FACE_OUTER_BOUND('',#3034,.T.);
#2284=FACE_OUTER_BOUND('',#3035,.T.);
#2285=FACE_OUTER_BOUND('',#3036,.T.);
#2286=FACE_OUTER_BOUND('',#3037,.T.);
#2287=FACE_OUTER_BOUND('',#3038,.T.);
#2288=FACE_OUTER_BOUND('',#3039,.T.);
#2289=FACE_OUTER_BOUND('',#3040,.T.);
#2290=FACE_OUTER_BOUND('',#3041,.T.);
#2291=FACE_OUTER_BOUND('',#3042,.T.);
#2292=FACE_OUTER_BOUND('',#3043,.T.);
#2293=FACE_OUTER_BOUND('',#3044,.T.);
#2294=FACE_OUTER_BOUND('',#3045,.T.);
#2295=FACE_OUTER_BOUND('',#3046,.T.);
#2296=FACE_OUTER_BOUND('',#3047,.T.);
#2297=FACE_OUTER_BOUND('',#3048,.T.);
#2298=FACE_OUTER_BOUND('',#3049,.T.);
#2299=FACE_OUTER_BOUND('',#3050,.T.);
#2300=FACE_OUTER_BOUND('',#3051,.T.);
#2301=FACE_OUTER_BOUND('',#3052,.T.);
#2302=FACE_OUTER_BOUND('',#3053,.T.);
#2303=FACE_OUTER_BOUND('',#3054,.T.);
#2304=FACE_OUTER_BOUND('',#3055,.T.);
#2305=FACE_OUTER_BOUND('',#3056,.T.);
#2306=FACE_OUTER_BOUND('',#3057,.T.);
#2307=FACE_OUTER_BOUND('',#3058,.T.);
#2308=FACE_OUTER_BOUND('',#3059,.T.);
#2309=FACE_OUTER_BOUND('',#3060,.T.);
#2310=FACE_OUTER_BOUND('',#3061,.T.);
#2311=FACE_OUTER_BOUND('',#3063,.T.);
#2312=FACE_OUTER_BOUND('',#3064,.T.);
#2313=FACE_OUTER_BOUND('',#3065,.T.);
#2314=FACE_OUTER_BOUND('',#3066,.T.);
#2315=FACE_OUTER_BOUND('',#3067,.T.);
#2316=FACE_OUTER_BOUND('',#3068,.T.);
#2317=FACE_OUTER_BOUND('',#3069,.T.);
#2318=FACE_OUTER_BOUND('',#3070,.T.);
#2319=FACE_OUTER_BOUND('',#3071,.T.);
#2320=FACE_OUTER_BOUND('',#3072,.T.);
#2321=FACE_OUTER_BOUND('',#3073,.T.);
#2322=FACE_OUTER_BOUND('',#3074,.T.);
#2323=FACE_OUTER_BOUND('',#3075,.T.);
#2324=FACE_OUTER_BOUND('',#3076,.T.);
#2325=FACE_OUTER_BOUND('',#3077,.T.);
#2326=FACE_OUTER_BOUND('',#3078,.T.);
#2327=FACE_OUTER_BOUND('',#3079,.T.);
#2328=FACE_OUTER_BOUND('',#3080,.T.);
#2329=FACE_OUTER_BOUND('',#3081,.T.);
#2330=FACE_OUTER_BOUND('',#3082,.T.);
#2331=FACE_OUTER_BOUND('',#3083,.T.);
#2332=FACE_OUTER_BOUND('',#3084,.T.);
#2333=FACE_OUTER_BOUND('',#3085,.T.);
#2334=FACE_OUTER_BOUND('',#3086,.T.);
#2335=FACE_OUTER_BOUND('',#3087,.T.);
#2336=FACE_OUTER_BOUND('',#3088,.T.);
#2337=FACE_OUTER_BOUND('',#3089,.T.);
#2338=FACE_OUTER_BOUND('',#3090,.T.);
#2339=FACE_OUTER_BOUND('',#3091,.T.);
#2340=FACE_OUTER_BOUND('',#3092,.T.);
#2341=FACE_OUTER_BOUND('',#3093,.T.);
#2342=FACE_OUTER_BOUND('',#3094,.T.);
#2343=FACE_OUTER_BOUND('',#3095,.T.);
#2344=FACE_OUTER_BOUND('',#3096,.T.);
#2345=FACE_OUTER_BOUND('',#3097,.T.);
#2346=FACE_OUTER_BOUND('',#3098,.T.);
#2347=FACE_OUTER_BOUND('',#3099,.T.);
#2348=FACE_OUTER_BOUND('',#3100,.T.);
#2349=FACE_OUTER_BOUND('',#3101,.T.);
#2350=FACE_OUTER_BOUND('',#3102,.T.);
#2351=FACE_OUTER_BOUND('',#3103,.T.);
#2352=FACE_OUTER_BOUND('',#3104,.T.);
#2353=FACE_OUTER_BOUND('',#3105,.T.);
#2354=FACE_OUTER_BOUND('',#3106,.T.);
#2355=FACE_OUTER_BOUND('',#3107,.T.);
#2356=FACE_OUTER_BOUND('',#3108,.T.);
#2357=FACE_OUTER_BOUND('',#3109,.T.);
#2358=FACE_OUTER_BOUND('',#3110,.T.);
#2359=FACE_OUTER_BOUND('',#3111,.T.);
#2360=FACE_OUTER_BOUND('',#3112,.T.);
#2361=FACE_OUTER_BOUND('',#3113,.T.);
#2362=FACE_OUTER_BOUND('',#3114,.T.);
#2363=FACE_OUTER_BOUND('',#3115,.T.);
#2364=FACE_OUTER_BOUND('',#3116,.T.);
#2365=FACE_OUTER_BOUND('',#3117,.T.);
#2366=FACE_OUTER_BOUND('',#3118,.T.);
#2367=FACE_OUTER_BOUND('',#3119,.T.);
#2368=FACE_OUTER_BOUND('',#3120,.T.);
#2369=FACE_OUTER_BOUND('',#3121,.T.);
#2370=FACE_OUTER_BOUND('',#3122,.T.);
#2371=FACE_OUTER_BOUND('',#3123,.T.);
#2372=FACE_OUTER_BOUND('',#3124,.T.);
#2373=FACE_OUTER_BOUND('',#3125,.T.);
#2374=FACE_OUTER_BOUND('',#3126,.T.);
#2375=FACE_OUTER_BOUND('',#3127,.T.);
#2376=FACE_OUTER_BOUND('',#3128,.T.);
#2377=FACE_OUTER_BOUND('',#3129,.T.);
#2378=FACE_OUTER_BOUND('',#3130,.T.);
#2379=FACE_OUTER_BOUND('',#3131,.T.);
#2380=FACE_OUTER_BOUND('',#3132,.T.);
#2381=FACE_OUTER_BOUND('',#3133,.T.);
#2382=FACE_OUTER_BOUND('',#3134,.T.);
#2383=FACE_OUTER_BOUND('',#3135,.T.);
#2384=FACE_OUTER_BOUND('',#3136,.T.);
#2385=FACE_OUTER_BOUND('',#3137,.T.);
#2386=FACE_OUTER_BOUND('',#3138,.T.);
#2387=FACE_OUTER_BOUND('',#3139,.T.);
#2388=FACE_OUTER_BOUND('',#3140,.T.);
#2389=FACE_OUTER_BOUND('',#3141,.T.);
#2390=FACE_OUTER_BOUND('',#3142,.T.);
#2391=FACE_OUTER_BOUND('',#3143,.T.);
#2392=FACE_OUTER_BOUND('',#3144,.T.);
#2393=FACE_OUTER_BOUND('',#3145,.T.);
#2394=FACE_OUTER_BOUND('',#3146,.T.);
#2395=FACE_OUTER_BOUND('',#3147,.T.);
#2396=FACE_OUTER_BOUND('',#3148,.T.);
#2397=FACE_OUTER_BOUND('',#3149,.T.);
#2398=FACE_OUTER_BOUND('',#3150,.T.);
#2399=FACE_OUTER_BOUND('',#3151,.T.);
#2400=FACE_OUTER_BOUND('',#3152,.T.);
#2401=FACE_OUTER_BOUND('',#3153,.T.);
#2402=FACE_OUTER_BOUND('',#3154,.T.);
#2403=FACE_OUTER_BOUND('',#3155,.T.);
#2404=FACE_OUTER_BOUND('',#3156,.T.);
#2405=FACE_OUTER_BOUND('',#3157,.T.);
#2406=FACE_OUTER_BOUND('',#3158,.T.);
#2407=FACE_OUTER_BOUND('',#3159,.T.);
#2408=FACE_OUTER_BOUND('',#3160,.T.);
#2409=FACE_OUTER_BOUND('',#3161,.T.);
#2410=FACE_OUTER_BOUND('',#3162,.T.);
#2411=FACE_OUTER_BOUND('',#3163,.T.);
#2412=FACE_OUTER_BOUND('',#3164,.T.);
#2413=FACE_OUTER_BOUND('',#3165,.T.);
#2414=FACE_OUTER_BOUND('',#3166,.T.);
#2415=FACE_OUTER_BOUND('',#3167,.T.);
#2416=FACE_OUTER_BOUND('',#3168,.T.);
#2417=FACE_OUTER_BOUND('',#3169,.T.);
#2418=FACE_OUTER_BOUND('',#3170,.T.);
#2419=FACE_OUTER_BOUND('',#3171,.T.);
#2420=FACE_OUTER_BOUND('',#3172,.T.);
#2421=FACE_OUTER_BOUND('',#3173,.T.);
#2422=FACE_OUTER_BOUND('',#3174,.T.);
#2423=FACE_OUTER_BOUND('',#3175,.T.);
#2424=FACE_OUTER_BOUND('',#3176,.T.);
#2425=FACE_OUTER_BOUND('',#3177,.T.);
#2426=FACE_OUTER_BOUND('',#3178,.T.);
#2427=FACE_OUTER_BOUND('',#3179,.T.);
#2428=FACE_OUTER_BOUND('',#3180,.T.);
#2429=FACE_OUTER_BOUND('',#3181,.T.);
#2430=FACE_OUTER_BOUND('',#3182,.T.);
#2431=FACE_OUTER_BOUND('',#3183,.T.);
#2432=FACE_OUTER_BOUND('',#3184,.T.);
#2433=FACE_OUTER_BOUND('',#3185,.T.);
#2434=FACE_OUTER_BOUND('',#3186,.T.);
#2435=FACE_OUTER_BOUND('',#3187,.T.);
#2436=FACE_OUTER_BOUND('',#3188,.T.);
#2437=FACE_OUTER_BOUND('',#3189,.T.);
#2438=FACE_OUTER_BOUND('',#3190,.T.);
#2439=FACE_OUTER_BOUND('',#3191,.T.);
#2440=FACE_OUTER_BOUND('',#3192,.T.);
#2441=FACE_OUTER_BOUND('',#3193,.T.);
#2442=FACE_OUTER_BOUND('',#3194,.T.);
#2443=FACE_OUTER_BOUND('',#3195,.T.);
#2444=FACE_OUTER_BOUND('',#3196,.T.);
#2445=FACE_OUTER_BOUND('',#3197,.T.);
#2446=FACE_OUTER_BOUND('',#3198,.T.);
#2447=FACE_OUTER_BOUND('',#3199,.T.);
#2448=FACE_OUTER_BOUND('',#3200,.T.);
#2449=FACE_OUTER_BOUND('',#3201,.T.);
#2450=FACE_OUTER_BOUND('',#3202,.T.);
#2451=FACE_OUTER_BOUND('',#3203,.T.);
#2452=FACE_OUTER_BOUND('',#3204,.T.);
#2453=FACE_OUTER_BOUND('',#3205,.T.);
#2454=FACE_OUTER_BOUND('',#3206,.T.);
#2455=FACE_OUTER_BOUND('',#3207,.T.);
#2456=FACE_OUTER_BOUND('',#3208,.T.);
#2457=FACE_OUTER_BOUND('',#3209,.T.);
#2458=FACE_OUTER_BOUND('',#3211,.T.);
#2459=FACE_OUTER_BOUND('',#3212,.T.);
#2460=FACE_OUTER_BOUND('',#3213,.T.);
#2461=FACE_OUTER_BOUND('',#3214,.T.);
#2462=FACE_OUTER_BOUND('',#3216,.T.);
#2463=FACE_OUTER_BOUND('',#3217,.T.);
#2464=FACE_OUTER_BOUND('',#3218,.T.);
#2465=FACE_OUTER_BOUND('',#3219,.T.);
#2466=FACE_OUTER_BOUND('',#3221,.T.);
#2467=FACE_OUTER_BOUND('',#3222,.T.);
#2468=FACE_OUTER_BOUND('',#3224,.T.);
#2469=FACE_OUTER_BOUND('',#3225,.T.);
#2470=FACE_OUTER_BOUND('',#3226,.T.);
#2471=FACE_OUTER_BOUND('',#3227,.T.);
#2472=FACE_OUTER_BOUND('',#3229,.T.);
#2473=FACE_OUTER_BOUND('',#3230,.T.);
#2474=FACE_OUTER_BOUND('',#3231,.T.);
#2475=FACE_OUTER_BOUND('',#3232,.T.);
#2476=FACE_OUTER_BOUND('',#3233,.T.);
#2477=FACE_OUTER_BOUND('',#3234,.T.);
#2478=FACE_OUTER_BOUND('',#3235,.T.);
#2479=FACE_OUTER_BOUND('',#3236,.T.);
#2480=FACE_OUTER_BOUND('',#3237,.T.);
#2481=FACE_OUTER_BOUND('',#3238,.T.);
#2482=FACE_OUTER_BOUND('',#3239,.T.);
#2483=FACE_OUTER_BOUND('',#3240,.T.);
#2484=FACE_OUTER_BOUND('',#3241,.T.);
#2485=FACE_OUTER_BOUND('',#3242,.T.);
#2486=FACE_OUTER_BOUND('',#3243,.T.);
#2487=FACE_OUTER_BOUND('',#3244,.T.);
#2488=FACE_OUTER_BOUND('',#3245,.T.);
#2489=FACE_OUTER_BOUND('',#3246,.T.);
#2490=FACE_OUTER_BOUND('',#3247,.T.);
#2491=FACE_OUTER_BOUND('',#3248,.T.);
#2492=FACE_OUTER_BOUND('',#3249,.T.);
#2493=FACE_OUTER_BOUND('',#3250,.T.);
#2494=FACE_OUTER_BOUND('',#3251,.T.);
#2495=FACE_OUTER_BOUND('',#3252,.T.);
#2496=FACE_OUTER_BOUND('',#3253,.T.);
#2497=FACE_OUTER_BOUND('',#3254,.T.);
#2498=FACE_OUTER_BOUND('',#3255,.T.);
#2499=FACE_OUTER_BOUND('',#3256,.T.);
#2500=FACE_OUTER_BOUND('',#3257,.T.);
#2501=FACE_OUTER_BOUND('',#3258,.T.);
#2502=FACE_OUTER_BOUND('',#3259,.T.);
#2503=FACE_OUTER_BOUND('',#3260,.T.);
#2504=FACE_OUTER_BOUND('',#3262,.T.);
#2505=FACE_OUTER_BOUND('',#3263,.T.);
#2506=FACE_OUTER_BOUND('',#3264,.T.);
#2507=FACE_OUTER_BOUND('',#3265,.T.);
#2508=FACE_OUTER_BOUND('',#3266,.T.);
#2509=FACE_OUTER_BOUND('',#3267,.T.);
#2510=FACE_OUTER_BOUND('',#3269,.T.);
#2511=FACE_OUTER_BOUND('',#3270,.T.);
#2512=FACE_OUTER_BOUND('',#3271,.T.);
#2513=EDGE_LOOP('',(#7753,#7754,#7755,#7756,#7757,#7758));
#2514=EDGE_LOOP('',(#7759,#7760,#7761,#7762,#7763,#7764));
#2515=EDGE_LOOP('',(#7765));
#2516=EDGE_LOOP('',(#7766,#7767,#7768,#7769,#7770));
#2517=EDGE_LOOP('',(#7771,#7772,#7773,#7774,#7775,#7776,#7777));
#2518=EDGE_LOOP('',(#7778,#7779,#7780,#7781,#7782,#7783));
#2519=EDGE_LOOP('',(#7784,#7785,#7786,#7787));
#2520=EDGE_LOOP('',(#7788,#7789,#7790,#7791,#7792,#7793));
#2521=EDGE_LOOP('',(#7794,#7795,#7796,#7797,#7798,#7799,#7800));
#2522=EDGE_LOOP('',(#7801,#7802,#7803,#7804,#7805,#7806));
#2523=EDGE_LOOP('',(#7807,#7808,#7809,#7810,#7811,#7812));
#2524=EDGE_LOOP('',(#7813,#7814,#7815,#7816,#7817,#7818,#7819));
#2525=EDGE_LOOP('',(#7820,#7821,#7822,#7823,#7824,#7825));
#2526=EDGE_LOOP('',(#7826,#7827,#7828,#7829));
#2527=EDGE_LOOP('',(#7830));
#2528=EDGE_LOOP('',(#7831,#7832,#7833,#7834,#7835,#7836));
#2529=EDGE_LOOP('',(#7837,#7838,#7839,#7840,#7841,#7842,#7843));
#2530=EDGE_LOOP('',(#7844,#7845,#7846,#7847,#7848,#7849));
#2531=EDGE_LOOP('',(#7850,#7851,#7852,#7853,#7854,#7855));
#2532=EDGE_LOOP('',(#7856,#7857,#7858,#7859,#7860,#7861,#7862));
#2533=EDGE_LOOP('',(#7863,#7864,#7865,#7866));
#2534=EDGE_LOOP('',(#7867,#7868,#7869,#7870,#7871,#7872));
#2535=EDGE_LOOP('',(#7873,#7874,#7875,#7876,#7877,#7878));
#2536=EDGE_LOOP('',(#7879,#7880,#7881,#7882,#7883,#7884));
#2537=EDGE_LOOP('',(#7885,#7886,#7887,#7888,#7889,#7890,#7891));
#2538=EDGE_LOOP('',(#7892,#7893,#7894,#7895,#7896,#7897));
#2539=EDGE_LOOP('',(#7898,#7899,#7900,#7901));
#2540=EDGE_LOOP('',(#7902));
#2541=EDGE_LOOP('',(#7903,#7904,#7905,#7906,#7907,#7908));
#2542=EDGE_LOOP('',(#7909,#7910,#7911,#7912));
#2543=EDGE_LOOP('',(#7913,#7914,#7915,#7916,#7917,#7918,#7919));
#2544=EDGE_LOOP('',(#7920,#7921,#7922,#7923,#7924,#7925));
#2545=EDGE_LOOP('',(#7926,#7927,#7928,#7929,#7930,#7931));
#2546=EDGE_LOOP('',(#7932,#7933,#7934,#7935,#7936,#7937,#7938));
#2547=EDGE_LOOP('',(#7939,#7940,#7941,#7942,#7943,#7944));
#2548=EDGE_LOOP('',(#7945,#7946,#7947,#7948));
#2549=EDGE_LOOP('',(#7949,#7950,#7951,#7952,#7953,#7954));
#2550=EDGE_LOOP('',(#7955,#7956,#7957,#7958,#7959,#7960,#7961));
#2551=EDGE_LOOP('',(#7962,#7963,#7964,#7965,#7966,#7967));
#2552=EDGE_LOOP('',(#7968,#7969,#7970,#7971,#7972,#7973));
#2553=EDGE_LOOP('',(#7974,#7975,#7976,#7977,#7978,#7979,#7980));
#2554=EDGE_LOOP('',(#7981,#7982,#7983,#7984,#7985,#7986));
#2555=EDGE_LOOP('',(#7987,#7988,#7989,#7990,#7991,#7992));
#2556=EDGE_LOOP('',(#7993));
#2557=EDGE_LOOP('',(#7994,#7995,#7996,#7997,#7998));
#2558=EDGE_LOOP('',(#7999,#8000,#8001,#8002,#8003,#8004,#8005));
#2559=EDGE_LOOP('',(#8006,#8007,#8008,#8009,#8010,#8011));
#2560=EDGE_LOOP('',(#8012,#8013,#8014,#8015,#8016));
#2561=EDGE_LOOP('',(#8017,#8018,#8019,#8020));
#2562=EDGE_LOOP('',(#8021,#8022,#8023));
#2563=EDGE_LOOP('',(#8024,#8025,#8026,#8027,#8028,#8029,#8030,#8031,#8032,
#8033,#8034,#8035,#8036,#8037,#8038,#8039));
#2564=EDGE_LOOP('',(#8040));
#2565=EDGE_LOOP('',(#8041));
#2566=EDGE_LOOP('',(#8042));
#2567=EDGE_LOOP('',(#8043));
#2568=EDGE_LOOP('',(#8044,#8045,#8046,#8047,#8048));
#2569=EDGE_LOOP('',(#8049,#8050,#8051,#8052,#8053,#8054));
#2570=EDGE_LOOP('',(#8055,#8056,#8057,#8058,#8059,#8060));
#2571=EDGE_LOOP('',(#8061,#8062,#8063,#8064,#8065,#8066));
#2572=EDGE_LOOP('',(#8067,#8068,#8069,#8070,#8071,#8072));
#2573=EDGE_LOOP('',(#8073,#8074,#8075,#8076,#8077));
#2574=EDGE_LOOP('',(#8078,#8079,#8080,#8081));
#2575=EDGE_LOOP('',(#8082,#8083,#8084));
#2576=EDGE_LOOP('',(#8085,#8086,#8087,#8088,#8089,#8090));
#2577=EDGE_LOOP('',(#8091,#8092,#8093,#8094,#8095));
#2578=EDGE_LOOP('',(#8096,#8097,#8098,#8099));
#2579=EDGE_LOOP('',(#8100,#8101,#8102));
#2580=EDGE_LOOP('',(#8103,#8104,#8105,#8106,#8107,#8108,#8109,#8110,#8111,
#8112,#8113,#8114,#8115,#8116,#8117,#8118));
#2581=EDGE_LOOP('',(#8119));
#2582=EDGE_LOOP('',(#8120));
#2583=EDGE_LOOP('',(#8121));
#2584=EDGE_LOOP('',(#8122));
#2585=EDGE_LOOP('',(#8123,#8124,#8125,#8126,#8127));
#2586=EDGE_LOOP('',(#8128,#8129,#8130,#8131,#8132,#8133));
#2587=EDGE_LOOP('',(#8134,#8135,#8136,#8137,#8138,#8139));
#2588=EDGE_LOOP('',(#8140,#8141,#8142,#8143,#8144,#8145,#8146));
#2589=EDGE_LOOP('',(#8147,#8148,#8149,#8150,#8151,#8152));
#2590=EDGE_LOOP('',(#8153,#8154,#8155,#8156,#8157,#8158));
#2591=EDGE_LOOP('',(#8159,#8160,#8161,#8162,#8163));
#2592=EDGE_LOOP('',(#8164,#8165,#8166,#8167));
#2593=EDGE_LOOP('',(#8168,#8169,#8170));
#2594=EDGE_LOOP('',(#8171,#8172,#8173,#8174));
#2595=EDGE_LOOP('',(#8175,#8176,#8177,#8178));
#2596=EDGE_LOOP('',(#8179,#8180,#8181,#8182));
#2597=EDGE_LOOP('',(#8183,#8184,#8185,#8186));
#2598=EDGE_LOOP('',(#8187,#8188,#8189,#8190));
#2599=EDGE_LOOP('',(#8191,#8192,#8193,#8194));
#2600=EDGE_LOOP('',(#8195,#8196,#8197,#8198));
#2601=EDGE_LOOP('',(#8199,#8200,#8201,#8202));
#2602=EDGE_LOOP('',(#8203,#8204,#8205,#8206));
#2603=EDGE_LOOP('',(#8207,#8208,#8209,#8210));
#2604=EDGE_LOOP('',(#8211,#8212,#8213,#8214));
#2605=EDGE_LOOP('',(#8215,#8216,#8217,#8218));
#2606=EDGE_LOOP('',(#8219,#8220,#8221,#8222));
#2607=EDGE_LOOP('',(#8223,#8224,#8225,#8226));
#2608=EDGE_LOOP('',(#8227));
#2609=EDGE_LOOP('',(#8228));
#2610=EDGE_LOOP('',(#8229,#8230,#8231,#8232));
#2611=EDGE_LOOP('',(#8233));
#2612=EDGE_LOOP('',(#8234));
#2613=EDGE_LOOP('',(#8235,#8236,#8237,#8238));
#2614=EDGE_LOOP('',(#8239,#8240,#8241,#8242));
#2615=EDGE_LOOP('',(#8243,#8244,#8245,#8246));
#2616=EDGE_LOOP('',(#8247,#8248,#8249,#8250));
#2617=EDGE_LOOP('',(#8251));
#2618=EDGE_LOOP('',(#8252));
#2619=EDGE_LOOP('',(#8253,#8254,#8255,#8256));
#2620=EDGE_LOOP('',(#8257));
#2621=EDGE_LOOP('',(#8258));
#2622=EDGE_LOOP('',(#8259,#8260,#8261,#8262));
#2623=EDGE_LOOP('',(#8263,#8264,#8265,#8266));
#2624=EDGE_LOOP('',(#8267,#8268,#8269,#8270));
#2625=EDGE_LOOP('',(#8271,#8272,#8273,#8274));
#2626=EDGE_LOOP('',(#8275));
#2627=EDGE_LOOP('',(#8276));
#2628=EDGE_LOOP('',(#8277,#8278,#8279,#8280));
#2629=EDGE_LOOP('',(#8281));
#2630=EDGE_LOOP('',(#8282));
#2631=EDGE_LOOP('',(#8283,#8284,#8285,#8286));
#2632=EDGE_LOOP('',(#8287,#8288,#8289,#8290));
#2633=EDGE_LOOP('',(#8291,#8292,#8293,#8294));
#2634=EDGE_LOOP('',(#8295,#8296,#8297,#8298));
#2635=EDGE_LOOP('',(#8299,#8300,#8301,#8302));
#2636=EDGE_LOOP('',(#8303,#8304,#8305,#8306));
#2637=EDGE_LOOP('',(#8307,#8308,#8309,#8310));
#2638=EDGE_LOOP('',(#8311,#8312,#8313,#8314));
#2639=EDGE_LOOP('',(#8315,#8316,#8317,#8318,#8319));
#2640=EDGE_LOOP('',(#8320,#8321,#8322,#8323,#8324,#8325));
#2641=EDGE_LOOP('',(#8326,#8327,#8328,#8329,#8330));
#2642=EDGE_LOOP('',(#8331,#8332,#8333,#8334));
#2643=EDGE_LOOP('',(#8335,#8336,#8337,#8338,#8339));
#2644=EDGE_LOOP('',(#8340,#8341,#8342,#8343));
#2645=EDGE_LOOP('',(#8344,#8345,#8346,#8347,#8348));
#2646=EDGE_LOOP('',(#8349,#8350,#8351));
#2647=EDGE_LOOP('',(#8352,#8353,#8354));
#2648=EDGE_LOOP('',(#8355,#8356,#8357));
#2649=EDGE_LOOP('',(#8358,#8359,#8360));
#2650=EDGE_LOOP('',(#8361,#8362,#8363,#8364,#8365,#8366));
#2651=EDGE_LOOP('',(#8367,#8368,#8369,#8370,#8371,#8372));
#2652=EDGE_LOOP('',(#8373,#8374,#8375,#8376));
#2653=EDGE_LOOP('',(#8377));
#2654=EDGE_LOOP('',(#8378,#8379,#8380,#8381,#8382,#8383));
#2655=EDGE_LOOP('',(#8384,#8385,#8386,#8387));
#2656=EDGE_LOOP('',(#8388,#8389,#8390,#8391,#8392,#8393));
#2657=EDGE_LOOP('',(#8394,#8395,#8396,#8397));
#2658=EDGE_LOOP('',(#8398,#8399,#8400,#8401));
#2659=EDGE_LOOP('',(#8402,#8403,#8404,#8405));
#2660=EDGE_LOOP('',(#8406));
#2661=EDGE_LOOP('',(#8407,#8408,#8409,#8410));
#2662=EDGE_LOOP('',(#8411,#8412,#8413,#8414,#8415));
#2663=EDGE_LOOP('',(#8416,#8417,#8418,#8419,#8420,#8421,#8422,#8423,#8424,
#8425,#8426,#8427,#8428,#8429,#8430,#8431,#8432,#8433,#8434,#8435,#8436,
#8437,#8438,#8439,#8440,#8441,#8442,#8443,#8444,#8445,#8446,#8447,#8448,
#8449,#8450,#8451,#8452,#8453,#8454,#8455,#8456,#8457,#8458,#8459,#8460,
#8461,#8462,#8463,#8464,#8465,#8466,#8467,#8468,#8469,#8470,#8471,#8472,
#8473,#8474,#8475,#8476,#8477,#8478,#8479,#8480,#8481,#8482,#8483,#8484,
#8485,#8486,#8487,#8488,#8489,#8490,#8491,#8492,#8493,#8494,#8495,#8496,
#8497,#8498,#8499,#8500));
#2664=EDGE_LOOP('',(#8501));
#2665=EDGE_LOOP('',(#8502,#8503,#8504,#8505));
#2666=EDGE_LOOP('',(#8506,#8507,#8508,#8509,#8510,#8511,#8512,#8513,#8514));
#2667=EDGE_LOOP('',(#8515,#8516,#8517,#8518,#8519));
#2668=EDGE_LOOP('',(#8520,#8521,#8522,#8523));
#2669=EDGE_LOOP('',(#8524,#8525,#8526,#8527,#8528,#8529));
#2670=EDGE_LOOP('',(#8530,#8531,#8532,#8533,#8534,#8535,#8536,#8537,#8538));
#2671=EDGE_LOOP('',(#8539,#8540,#8541,#8542,#8543,#8544));
#2672=EDGE_LOOP('',(#8545,#8546,#8547,#8548,#8549,#8550,#8551,#8552,#8553,
#8554));
#2673=EDGE_LOOP('',(#8555,#8556,#8557,#8558));
#2674=EDGE_LOOP('',(#8559,#8560,#8561,#8562));
#2675=EDGE_LOOP('',(#8563,#8564,#8565,#8566));
#2676=EDGE_LOOP('',(#8567,#8568,#8569,#8570));
#2677=EDGE_LOOP('',(#8571,#8572,#8573,#8574));
#2678=EDGE_LOOP('',(#8575,#8576,#8577,#8578));
#2679=EDGE_LOOP('',(#8579,#8580,#8581,#8582));
#2680=EDGE_LOOP('',(#8583,#8584,#8585,#8586));
#2681=EDGE_LOOP('',(#8587,#8588,#8589,#8590));
#2682=EDGE_LOOP('',(#8591,#8592,#8593,#8594));
#2683=EDGE_LOOP('',(#8595,#8596,#8597,#8598));
#2684=EDGE_LOOP('',(#8599,#8600,#8601,#8602));
#2685=EDGE_LOOP('',(#8603,#8604,#8605,#8606));
#2686=EDGE_LOOP('',(#8607,#8608,#8609,#8610));
#2687=EDGE_LOOP('',(#8611,#8612,#8613,#8614));
#2688=EDGE_LOOP('',(#8615,#8616,#8617,#8618));
#2689=EDGE_LOOP('',(#8619,#8620,#8621,#8622));
#2690=EDGE_LOOP('',(#8623,#8624,#8625,#8626));
#2691=EDGE_LOOP('',(#8627,#8628,#8629,#8630));
#2692=EDGE_LOOP('',(#8631,#8632,#8633,#8634));
#2693=EDGE_LOOP('',(#8635,#8636,#8637,#8638));
#2694=EDGE_LOOP('',(#8639,#8640,#8641,#8642));
#2695=EDGE_LOOP('',(#8643,#8644,#8645,#8646));
#2696=EDGE_LOOP('',(#8647,#8648,#8649,#8650));
#2697=EDGE_LOOP('',(#8651,#8652,#8653,#8654));
#2698=EDGE_LOOP('',(#8655,#8656,#8657,#8658));
#2699=EDGE_LOOP('',(#8659,#8660,#8661,#8662));
#2700=EDGE_LOOP('',(#8663,#8664,#8665,#8666));
#2701=EDGE_LOOP('',(#8667,#8668,#8669,#8670));
#2702=EDGE_LOOP('',(#8671,#8672,#8673,#8674));
#2703=EDGE_LOOP('',(#8675,#8676,#8677,#8678));
#2704=EDGE_LOOP('',(#8679,#8680,#8681,#8682));
#2705=EDGE_LOOP('',(#8683,#8684,#8685,#8686));
#2706=EDGE_LOOP('',(#8687,#8688,#8689,#8690,#8691));
#2707=EDGE_LOOP('',(#8692,#8693,#8694,#8695));
#2708=EDGE_LOOP('',(#8696,#8697,#8698,#8699));
#2709=EDGE_LOOP('',(#8700,#8701,#8702,#8703));
#2710=EDGE_LOOP('',(#8704,#8705,#8706,#8707,#8708));
#2711=EDGE_LOOP('',(#8709,#8710,#8711,#8712));
#2712=EDGE_LOOP('',(#8713,#8714,#8715,#8716));
#2713=EDGE_LOOP('',(#8717,#8718,#8719,#8720));
#2714=EDGE_LOOP('',(#8721,#8722,#8723,#8724));
#2715=EDGE_LOOP('',(#8725,#8726,#8727,#8728));
#2716=EDGE_LOOP('',(#8729,#8730,#8731,#8732));
#2717=EDGE_LOOP('',(#8733,#8734,#8735,#8736));
#2718=EDGE_LOOP('',(#8737,#8738,#8739,#8740));
#2719=EDGE_LOOP('',(#8741,#8742,#8743,#8744));
#2720=EDGE_LOOP('',(#8745,#8746,#8747,#8748));
#2721=EDGE_LOOP('',(#8749,#8750,#8751,#8752));
#2722=EDGE_LOOP('',(#8753,#8754,#8755,#8756));
#2723=EDGE_LOOP('',(#8757,#8758,#8759,#8760));
#2724=EDGE_LOOP('',(#8761,#8762,#8763,#8764));
#2725=EDGE_LOOP('',(#8765,#8766,#8767,#8768));
#2726=EDGE_LOOP('',(#8769,#8770,#8771,#8772));
#2727=EDGE_LOOP('',(#8773,#8774,#8775,#8776));
#2728=EDGE_LOOP('',(#8777,#8778,#8779,#8780));
#2729=EDGE_LOOP('',(#8781,#8782,#8783,#8784));
#2730=EDGE_LOOP('',(#8785,#8786,#8787,#8788));
#2731=EDGE_LOOP('',(#8789,#8790,#8791,#8792));
#2732=EDGE_LOOP('',(#8793,#8794,#8795,#8796));
#2733=EDGE_LOOP('',(#8797,#8798,#8799,#8800));
#2734=EDGE_LOOP('',(#8801,#8802,#8803,#8804));
#2735=EDGE_LOOP('',(#8805,#8806,#8807,#8808));
#2736=EDGE_LOOP('',(#8809,#8810,#8811,#8812));
#2737=EDGE_LOOP('',(#8813,#8814,#8815,#8816));
#2738=EDGE_LOOP('',(#8817,#8818,#8819,#8820));
#2739=EDGE_LOOP('',(#8821,#8822,#8823,#8824));
#2740=EDGE_LOOP('',(#8825,#8826,#8827,#8828));
#2741=EDGE_LOOP('',(#8829,#8830,#8831,#8832));
#2742=EDGE_LOOP('',(#8833,#8834,#8835,#8836));
#2743=EDGE_LOOP('',(#8837,#8838,#8839,#8840));
#2744=EDGE_LOOP('',(#8841,#8842,#8843,#8844));
#2745=EDGE_LOOP('',(#8845,#8846,#8847,#8848));
#2746=EDGE_LOOP('',(#8849,#8850,#8851,#8852));
#2747=EDGE_LOOP('',(#8853,#8854,#8855,#8856));
#2748=EDGE_LOOP('',(#8857,#8858,#8859,#8860));
#2749=EDGE_LOOP('',(#8861,#8862,#8863,#8864));
#2750=EDGE_LOOP('',(#8865,#8866,#8867,#8868));
#2751=EDGE_LOOP('',(#8869,#8870,#8871,#8872));
#2752=EDGE_LOOP('',(#8873,#8874,#8875,#8876,#8877,#8878,#8879,#8880,#8881,
#8882,#8883,#8884,#8885,#8886,#8887,#8888,#8889,#8890,#8891,#8892,#8893,
#8894,#8895,#8896,#8897,#8898,#8899,#8900,#8901,#8902,#8903,#8904,#8905,
#8906,#8907,#8908,#8909,#8910,#8911,#8912,#8913,#8914,#8915,#8916,#8917,
#8918,#8919,#8920,#8921,#8922,#8923,#8924,#8925,#8926,#8927,#8928,#8929,
#8930,#8931,#8932,#8933,#8934,#8935,#8936,#8937,#8938,#8939,#8940,#8941,
#8942,#8943,#8944,#8945,#8946,#8947,#8948,#8949,#8950,#8951,#8952,#8953,
#8954,#8955,#8956));
#2753=EDGE_LOOP('',(#8957,#8958,#8959,#8960));
#2754=EDGE_LOOP('',(#8961));
#2755=EDGE_LOOP('',(#8962));
#2756=EDGE_LOOP('',(#8963,#8964,#8965,#8966));
#2757=EDGE_LOOP('',(#8967,#8968,#8969,#8970));
#2758=EDGE_LOOP('',(#8971,#8972));
#2759=EDGE_LOOP('',(#8973,#8974));
#2760=EDGE_LOOP('',(#8975,#8976,#8977,#8978));
#2761=EDGE_LOOP('',(#8979));
#2762=EDGE_LOOP('',(#8980));
#2763=EDGE_LOOP('',(#8981,#8982,#8983,#8984,#8985));
#2764=EDGE_LOOP('',(#8986,#8987,#8988,#8989,#8990));
#2765=EDGE_LOOP('',(#8991));
#2766=EDGE_LOOP('',(#8992));
#2767=EDGE_LOOP('',(#8993,#8994,#8995));
#2768=EDGE_LOOP('',(#8996,#8997));
#2769=EDGE_LOOP('',(#8998,#8999));
#2770=EDGE_LOOP('',(#9000,#9001,#9002,#9003));
#2771=EDGE_LOOP('',(#9004,#9005));
#2772=EDGE_LOOP('',(#9006,#9007,#9008,#9009));
#2773=EDGE_LOOP('',(#9010,#9011));
#2774=EDGE_LOOP('',(#9012));
#2775=EDGE_LOOP('',(#9013,#9014,#9015,#9016));
#2776=EDGE_LOOP('',(#9017,#9018,#9019,#9020));
#2777=EDGE_LOOP('',(#9021,#9022,#9023,#9024));
#2778=EDGE_LOOP('',(#9025,#9026,#9027,#9028));
#2779=EDGE_LOOP('',(#9029));
#2780=EDGE_LOOP('',(#9030));
#2781=EDGE_LOOP('',(#9031,#9032,#9033,#9034));
#2782=EDGE_LOOP('',(#9035));
#2783=EDGE_LOOP('',(#9036));
#2784=EDGE_LOOP('',(#9037,#9038,#9039,#9040));
#2785=EDGE_LOOP('',(#9041,#9042,#9043,#9044));
#2786=EDGE_LOOP('',(#9045,#9046,#9047,#9048,#9049,#9050,#9051,#9052,#9053));
#2787=EDGE_LOOP('',(#9054,#9055,#9056,#9057,#9058));
#2788=EDGE_LOOP('',(#9059,#9060,#9061,#9062));
#2789=EDGE_LOOP('',(#9063,#9064,#9065,#9066,#9067,#9068));
#2790=EDGE_LOOP('',(#9069,#9070,#9071,#9072,#9073,#9074,#9075,#9076,#9077));
#2791=EDGE_LOOP('',(#9078,#9079,#9080,#9081,#9082,#9083));
#2792=EDGE_LOOP('',(#9084,#9085,#9086,#9087,#9088,#9089,#9090,#9091,#9092,
#9093));
#2793=EDGE_LOOP('',(#9094,#9095,#9096,#9097));
#2794=EDGE_LOOP('',(#9098,#9099,#9100,#9101));
#2795=EDGE_LOOP('',(#9102,#9103,#9104,#9105));
#2796=EDGE_LOOP('',(#9106,#9107,#9108,#9109,#9110,#9111,#9112,#9113,#9114,
#9115,#9116,#9117,#9118,#9119,#9120,#9121,#9122,#9123,#9124,#9125,#9126,
#9127,#9128,#9129,#9130,#9131,#9132,#9133,#9134,#9135,#9136,#9137,#9138,
#9139,#9140,#9141,#9142,#9143,#9144,#9145,#9146,#9147,#9148,#9149,#9150,
#9151,#9152,#9153,#9154,#9155,#9156,#9157,#9158,#9159,#9160,#9161,#9162,
#9163,#9164,#9165,#9166,#9167,#9168,#9169,#9170,#9171,#9172,#9173,#9174,
#9175,#9176,#9177,#9178,#9179,#9180,#9181,#9182,#9183,#9184,#9185,#9186,
#9187,#9188,#9189));
#2797=EDGE_LOOP('',(#9190,#9191,#9192,#9193));
#2798=EDGE_LOOP('',(#9194,#9195,#9196,#9197));
#2799=EDGE_LOOP('',(#9198,#9199,#9200,#9201));
#2800=EDGE_LOOP('',(#9202,#9203,#9204,#9205));
#2801=EDGE_LOOP('',(#9206,#9207,#9208,#9209));
#2802=EDGE_LOOP('',(#9210,#9211,#9212,#9213));
#2803=EDGE_LOOP('',(#9214,#9215,#9216,#9217));
#2804=EDGE_LOOP('',(#9218,#9219,#9220,#9221));
#2805=EDGE_LOOP('',(#9222,#9223,#9224,#9225));
#2806=EDGE_LOOP('',(#9226,#9227,#9228,#9229));
#2807=EDGE_LOOP('',(#9230,#9231,#9232,#9233));
#2808=EDGE_LOOP('',(#9234,#9235,#9236,#9237));
#2809=EDGE_LOOP('',(#9238,#9239,#9240,#9241));
#2810=EDGE_LOOP('',(#9242,#9243,#9244,#9245));
#2811=EDGE_LOOP('',(#9246,#9247,#9248,#9249));
#2812=EDGE_LOOP('',(#9250,#9251,#9252,#9253));
#2813=EDGE_LOOP('',(#9254,#9255,#9256,#9257));
#2814=EDGE_LOOP('',(#9258,#9259,#9260,#9261));
#2815=EDGE_LOOP('',(#9262,#9263,#9264,#9265));
#2816=EDGE_LOOP('',(#9266,#9267,#9268,#9269));
#2817=EDGE_LOOP('',(#9270,#9271,#9272,#9273));
#2818=EDGE_LOOP('',(#9274,#9275,#9276,#9277));
#2819=EDGE_LOOP('',(#9278,#9279,#9280,#9281));
#2820=EDGE_LOOP('',(#9282,#9283,#9284,#9285));
#2821=EDGE_LOOP('',(#9286,#9287,#9288,#9289));
#2822=EDGE_LOOP('',(#9290,#9291,#9292,#9293));
#2823=EDGE_LOOP('',(#9294,#9295,#9296,#9297));
#2824=EDGE_LOOP('',(#9298,#9299,#9300,#9301));
#2825=EDGE_LOOP('',(#9302,#9303,#9304,#9305));
#2826=EDGE_LOOP('',(#9306,#9307,#9308,#9309));
#2827=EDGE_LOOP('',(#9310,#9311,#9312,#9313));
#2828=EDGE_LOOP('',(#9314,#9315,#9316,#9317));
#2829=EDGE_LOOP('',(#9318,#9319,#9320,#9321));
#2830=EDGE_LOOP('',(#9322,#9323,#9324,#9325));
#2831=EDGE_LOOP('',(#9326,#9327,#9328,#9329));
#2832=EDGE_LOOP('',(#9330,#9331,#9332,#9333,#9334));
#2833=EDGE_LOOP('',(#9335,#9336,#9337,#9338));
#2834=EDGE_LOOP('',(#9339,#9340,#9341,#9342));
#2835=EDGE_LOOP('',(#9343,#9344,#9345,#9346));
#2836=EDGE_LOOP('',(#9347,#9348,#9349,#9350,#9351));
#2837=EDGE_LOOP('',(#9352,#9353,#9354,#9355));
#2838=EDGE_LOOP('',(#9356,#9357,#9358,#9359));
#2839=EDGE_LOOP('',(#9360,#9361,#9362,#9363));
#2840=EDGE_LOOP('',(#9364,#9365,#9366,#9367));
#2841=EDGE_LOOP('',(#9368,#9369,#9370,#9371));
#2842=EDGE_LOOP('',(#9372,#9373,#9374,#9375));
#2843=EDGE_LOOP('',(#9376,#9377,#9378,#9379));
#2844=EDGE_LOOP('',(#9380,#9381,#9382,#9383));
#2845=EDGE_LOOP('',(#9384,#9385,#9386,#9387));
#2846=EDGE_LOOP('',(#9388,#9389,#9390,#9391));
#2847=EDGE_LOOP('',(#9392,#9393,#9394,#9395));
#2848=EDGE_LOOP('',(#9396,#9397,#9398,#9399));
#2849=EDGE_LOOP('',(#9400,#9401,#9402,#9403));
#2850=EDGE_LOOP('',(#9404,#9405,#9406,#9407));
#2851=EDGE_LOOP('',(#9408,#9409,#9410,#9411));
#2852=EDGE_LOOP('',(#9412,#9413,#9414,#9415));
#2853=EDGE_LOOP('',(#9416,#9417,#9418,#9419));
#2854=EDGE_LOOP('',(#9420,#9421,#9422,#9423));
#2855=EDGE_LOOP('',(#9424,#9425,#9426,#9427));
#2856=EDGE_LOOP('',(#9428,#9429,#9430,#9431));
#2857=EDGE_LOOP('',(#9432,#9433,#9434,#9435));
#2858=EDGE_LOOP('',(#9436,#9437,#9438,#9439));
#2859=EDGE_LOOP('',(#9440,#9441,#9442,#9443));
#2860=EDGE_LOOP('',(#9444,#9445,#9446,#9447));
#2861=EDGE_LOOP('',(#9448,#9449,#9450,#9451));
#2862=EDGE_LOOP('',(#9452,#9453,#9454,#9455));
#2863=EDGE_LOOP('',(#9456,#9457,#9458,#9459));
#2864=EDGE_LOOP('',(#9460,#9461,#9462,#9463));
#2865=EDGE_LOOP('',(#9464,#9465,#9466,#9467));
#2866=EDGE_LOOP('',(#9468,#9469,#9470,#9471));
#2867=EDGE_LOOP('',(#9472,#9473,#9474,#9475));
#2868=EDGE_LOOP('',(#9476,#9477,#9478,#9479));
#2869=EDGE_LOOP('',(#9480,#9481,#9482,#9483));
#2870=EDGE_LOOP('',(#9484,#9485,#9486,#9487));
#2871=EDGE_LOOP('',(#9488,#9489,#9490,#9491));
#2872=EDGE_LOOP('',(#9492,#9493,#9494,#9495));
#2873=EDGE_LOOP('',(#9496,#9497,#9498,#9499,#9500,#9501,#9502,#9503,#9504,
#9505,#9506,#9507,#9508,#9509,#9510,#9511,#9512,#9513,#9514,#9515,#9516,
#9517,#9518,#9519,#9520,#9521,#9522,#9523,#9524,#9525,#9526,#9527,#9528,
#9529,#9530,#9531,#9532,#9533,#9534,#9535,#9536,#9537,#9538,#9539,#9540,
#9541,#9542,#9543,#9544,#9545,#9546,#9547,#9548,#9549,#9550,#9551,#9552,
#9553,#9554,#9555,#9556,#9557,#9558,#9559,#9560,#9561,#9562,#9563,#9564,
#9565,#9566,#9567,#9568,#9569,#9570,#9571,#9572,#9573,#9574,#9575,#9576,
#9577,#9578,#9579));
#2874=EDGE_LOOP('',(#9580,#9581,#9582,#9583));
#2875=EDGE_LOOP('',(#9584));
#2876=EDGE_LOOP('',(#9585,#9586,#9587,#9588));
#2877=EDGE_LOOP('',(#9589));
#2878=EDGE_LOOP('',(#9590));
#2879=EDGE_LOOP('',(#9591,#9592,#9593,#9594));
#2880=EDGE_LOOP('',(#9595,#9596,#9597,#9598));
#2881=EDGE_LOOP('',(#9599,#9600));
#2882=EDGE_LOOP('',(#9601,#9602));
#2883=EDGE_LOOP('',(#9603,#9604,#9605,#9606));
#2884=EDGE_LOOP('',(#9607));
#2885=EDGE_LOOP('',(#9608));
#2886=EDGE_LOOP('',(#9609));
#2887=EDGE_LOOP('',(#9610));
#2888=EDGE_LOOP('',(#9611));
#2889=EDGE_LOOP('',(#9612));
#2890=EDGE_LOOP('',(#9613,#9614,#9615,#9616));
#2891=EDGE_LOOP('',(#9617,#9618,#9619,#9620));
#2892=EDGE_LOOP('',(#9621));
#2893=EDGE_LOOP('',(#9622));
#2894=EDGE_LOOP('',(#9623));
#2895=EDGE_LOOP('',(#9624));
#2896=EDGE_LOOP('',(#9625,#9626,#9627,#9628));
#2897=EDGE_LOOP('',(#9629,#9630,#9631,#9632,#9633,#9634,#9635,#9636,#9637,
#9638,#9639,#9640,#9641,#9642,#9643,#9644,#9645,#9646));
#2898=EDGE_LOOP('',(#9647,#9648,#9649,#9650,#9651,#9652,#9653,#9654,#9655,
#9656));
#2899=EDGE_LOOP('',(#9657,#9658,#9659,#9660));
#2900=EDGE_LOOP('',(#9661,#9662,#9663,#9664,#9665,#9666,#9667,#9668,#9669,
#9670,#9671,#9672,#9673,#9674,#9675,#9676,#9677,#9678));
#2901=EDGE_LOOP('',(#9679,#9680,#9681,#9682));
#2902=EDGE_LOOP('',(#9683,#9684,#9685,#9686,#9687,#9688,#9689,#9690,#9691,
#9692,#9693,#9694,#9695,#9696,#9697,#9698,#9699,#9700,#9701,#9702,#9703,
#9704,#9705,#9706,#9707));
#2903=EDGE_LOOP('',(#9708,#9709,#9710,#9711));
#2904=EDGE_LOOP('',(#9712,#9713,#9714,#9715,#9716,#9717,#9718,#9719,#9720,
#9721));
#2905=EDGE_LOOP('',(#9722,#9723,#9724,#9725));
#2906=EDGE_LOOP('',(#9726,#9727,#9728,#9729));
#2907=EDGE_LOOP('',(#9730,#9731,#9732,#9733));
#2908=EDGE_LOOP('',(#9734,#9735,#9736,#9737,#9738,#9739,#9740,#9741,#9742,
#9743));
#2909=EDGE_LOOP('',(#9744,#9745,#9746,#9747));
#2910=EDGE_LOOP('',(#9748,#9749,#9750,#9751,#9752,#9753));
#2911=EDGE_LOOP('',(#9754,#9755,#9756,#9757,#9758,#9759));
#2912=EDGE_LOOP('',(#9760,#9761,#9762,#9763,#9764,#9765,#9766,#9767,#9768,
#9769));
#2913=EDGE_LOOP('',(#9770,#9771,#9772,#9773));
#2914=EDGE_LOOP('',(#9774,#9775,#9776,#9777));
#2915=EDGE_LOOP('',(#9778,#9779,#9780,#9781));
#2916=EDGE_LOOP('',(#9782,#9783,#9784,#9785,#9786,#9787,#9788,#9789,#9790,
#9791));
#2917=EDGE_LOOP('',(#9792,#9793,#9794,#9795));
#2918=EDGE_LOOP('',(#9796,#9797,#9798,#9799));
#2919=EDGE_LOOP('',(#9800,#9801,#9802,#9803));
#2920=EDGE_LOOP('',(#9804,#9805,#9806,#9807,#9808,#9809,#9810,#9811,#9812,
#9813));
#2921=EDGE_LOOP('',(#9814,#9815,#9816,#9817));
#2922=EDGE_LOOP('',(#9818,#9819,#9820,#9821));
#2923=EDGE_LOOP('',(#9822,#9823,#9824,#9825));
#2924=EDGE_LOOP('',(#9826,#9827,#9828,#9829,#9830,#9831,#9832,#9833,#9834,
#9835,#9836,#9837,#9838,#9839,#9840,#9841,#9842,#9843,#9844,#9845,#9846,
#9847,#9848,#9849,#9850));
#2925=EDGE_LOOP('',(#9851,#9852,#9853,#9854));
#2926=EDGE_LOOP('',(#9855,#9856,#9857,#9858,#9859,#9860,#9861,#9862,#9863,
#9864));
#2927=EDGE_LOOP('',(#9865,#9866,#9867,#9868));
#2928=EDGE_LOOP('',(#9869,#9870,#9871,#9872));
#2929=EDGE_LOOP('',(#9873));
#2930=EDGE_LOOP('',(#9874));
#2931=EDGE_LOOP('',(#9875,#9876,#9877,#9878));
#2932=EDGE_LOOP('',(#9879,#9880,#9881,#9882));
#2933=EDGE_LOOP('',(#9883,#9884,#9885,#9886));
#2934=EDGE_LOOP('',(#9887));
#2935=EDGE_LOOP('',(#9888));
#2936=EDGE_LOOP('',(#9889,#9890,#9891,#9892));
#2937=EDGE_LOOP('',(#9893,#9894,#9895,#9896));
#2938=EDGE_LOOP('',(#9897,#9898,#9899,#9900));
#2939=EDGE_LOOP('',(#9901));
#2940=EDGE_LOOP('',(#9902));
#2941=EDGE_LOOP('',(#9903));
#2942=EDGE_LOOP('',(#9904));
#2943=EDGE_LOOP('',(#9905,#9906,#9907,#9908));
#2944=EDGE_LOOP('',(#9909,#9910,#9911,#9912));
#2945=EDGE_LOOP('',(#9913));
#2946=EDGE_LOOP('',(#9914));
#2947=EDGE_LOOP('',(#9915,#9916,#9917,#9918));
#2948=EDGE_LOOP('',(#9919));
#2949=EDGE_LOOP('',(#9920));
#2950=EDGE_LOOP('',(#9921,#9922,#9923,#9924));
#2951=EDGE_LOOP('',(#9925,#9926,#9927,#9928));
#2952=EDGE_LOOP('',(#9929,#9930,#9931,#9932,#9933,#9934));
#2953=EDGE_LOOP('',(#9935,#9936,#9937,#9938));
#2954=EDGE_LOOP('',(#9939,#9940,#9941,#9942));
#2955=EDGE_LOOP('',(#9943,#9944,#9945,#9946,#9947,#9948,#9949,#9950));
#2956=EDGE_LOOP('',(#9951,#9952,#9953,#9954));
#2957=EDGE_LOOP('',(#9955,#9956,#9957,#9958,#9959,#9960,#9961,#9962,#9963,
#9964));
#2958=EDGE_LOOP('',(#9965));
#2959=EDGE_LOOP('',(#9966));
#2960=EDGE_LOOP('',(#9967,#9968,#9969,#9970));
#2961=EDGE_LOOP('',(#9971,#9972,#9973,#9974,#9975,#9976));
#2962=EDGE_LOOP('',(#9977,#9978,#9979,#9980));
#2963=EDGE_LOOP('',(#9981,#9982,#9983,#9984));
#2964=EDGE_LOOP('',(#9985,#9986,#9987,#9988));
#2965=EDGE_LOOP('',(#9989,#9990,#9991,#9992));
#2966=EDGE_LOOP('',(#9993,#9994,#9995,#9996));
#2967=EDGE_LOOP('',(#9997,#9998,#9999,#10000));
#2968=EDGE_LOOP('',(#10001,#10002,#10003,#10004,#10005,#10006,#10007,#10008,
#10009,#10010));
#2969=EDGE_LOOP('',(#10011));
#2970=EDGE_LOOP('',(#10012));
#2971=EDGE_LOOP('',(#10013,#10014,#10015,#10016));
#2972=EDGE_LOOP('',(#10017,#10018,#10019,#10020));
#2973=EDGE_LOOP('',(#10021,#10022,#10023,#10024));
#2974=EDGE_LOOP('',(#10025,#10026,#10027,#10028));
#2975=EDGE_LOOP('',(#10029,#10030,#10031,#10032));
#2976=EDGE_LOOP('',(#10033,#10034,#10035,#10036));
#2977=EDGE_LOOP('',(#10037,#10038,#10039,#10040));
#2978=EDGE_LOOP('',(#10041,#10042,#10043));
#2979=EDGE_LOOP('',(#10044,#10045,#10046,#10047,#10048));
#2980=EDGE_LOOP('',(#10049,#10050,#10051,#10052));
#2981=EDGE_LOOP('',(#10053,#10054,#10055,#10056));
#2982=EDGE_LOOP('',(#10057,#10058,#10059,#10060));
#2983=EDGE_LOOP('',(#10061,#10062,#10063,#10064));
#2984=EDGE_LOOP('',(#10065,#10066,#10067,#10068,#10069,#10070));
#2985=EDGE_LOOP('',(#10071,#10072,#10073,#10074,#10075,#10076,#10077,#10078,
#10079,#10080,#10081,#10082,#10083,#10084,#10085));
#2986=EDGE_LOOP('',(#10086,#10087,#10088,#10089,#10090));
#2987=EDGE_LOOP('',(#10091,#10092,#10093,#10094));
#2988=EDGE_LOOP('',(#10095,#10096,#10097,#10098,#10099,#10100,#10101,#10102,
#10103,#10104,#10105,#10106,#10107,#10108,#10109,#10110));
#2989=EDGE_LOOP('',(#10111,#10112,#10113,#10114));
#2990=EDGE_LOOP('',(#10115,#10116,#10117,#10118));
#2991=EDGE_LOOP('',(#10119,#10120,#10121,#10122));
#2992=EDGE_LOOP('',(#10123,#10124,#10125,#10126));
#2993=EDGE_LOOP('',(#10127,#10128,#10129,#10130));
#2994=EDGE_LOOP('',(#10131,#10132,#10133,#10134));
#2995=EDGE_LOOP('',(#10135,#10136,#10137,#10138,#10139,#10140));
#2996=EDGE_LOOP('',(#10141));
#2997=EDGE_LOOP('',(#10142,#10143,#10144,#10145,#10146,#10147));
#2998=EDGE_LOOP('',(#10148,#10149,#10150,#10151,#10152,#10153));
#2999=EDGE_LOOP('',(#10154,#10155,#10156,#10157));
#3000=EDGE_LOOP('',(#10158,#10159,#10160,#10161,#10162,#10163));
#3001=EDGE_LOOP('',(#10164));
#3002=EDGE_LOOP('',(#10165,#10166,#10167,#10168));
#3003=EDGE_LOOP('',(#10169,#10170,#10171,#10172));
#3004=EDGE_LOOP('',(#10173,#10174,#10175,#10176));
#3005=EDGE_LOOP('',(#10177,#10178,#10179,#10180));
#3006=EDGE_LOOP('',(#10181,#10182,#10183,#10184));
#3007=EDGE_LOOP('',(#10185,#10186,#10187,#10188));
#3008=EDGE_LOOP('',(#10189,#10190,#10191,#10192));
#3009=EDGE_LOOP('',(#10193,#10194,#10195,#10196));
#3010=EDGE_LOOP('',(#10197,#10198,#10199,#10200));
#3011=EDGE_LOOP('',(#10201,#10202,#10203,#10204));
#3012=EDGE_LOOP('',(#10205,#10206,#10207,#10208));
#3013=EDGE_LOOP('',(#10209,#10210,#10211,#10212));
#3014=EDGE_LOOP('',(#10213,#10214,#10215,#10216));
#3015=EDGE_LOOP('',(#10217,#10218,#10219,#10220));
#3016=EDGE_LOOP('',(#10221,#10222,#10223,#10224));
#3017=EDGE_LOOP('',(#10225,#10226,#10227,#10228));
#3018=EDGE_LOOP('',(#10229,#10230,#10231,#10232));
#3019=EDGE_LOOP('',(#10233,#10234,#10235,#10236));
#3020=EDGE_LOOP('',(#10237,#10238,#10239,#10240));
#3021=EDGE_LOOP('',(#10241,#10242,#10243,#10244));
#3022=EDGE_LOOP('',(#10245,#10246,#10247,#10248));
#3023=EDGE_LOOP('',(#10249,#10250,#10251,#10252));
#3024=EDGE_LOOP('',(#10253,#10254,#10255,#10256));
#3025=EDGE_LOOP('',(#10257,#10258,#10259,#10260));
#3026=EDGE_LOOP('',(#10261,#10262,#10263));
#3027=EDGE_LOOP('',(#10264,#10265,#10266,#10267,#10268));
#3028=EDGE_LOOP('',(#10269,#10270,#10271,#10272));
#3029=EDGE_LOOP('',(#10273,#10274,#10275,#10276));
#3030=EDGE_LOOP('',(#10277,#10278,#10279,#10280));
#3031=EDGE_LOOP('',(#10281,#10282,#10283,#10284));
#3032=EDGE_LOOP('',(#10285,#10286,#10287,#10288));
#3033=EDGE_LOOP('',(#10289,#10290,#10291,#10292));
#3034=EDGE_LOOP('',(#10293,#10294,#10295,#10296));
#3035=EDGE_LOOP('',(#10297,#10298,#10299,#10300));
#3036=EDGE_LOOP('',(#10301,#10302,#10303,#10304));
#3037=EDGE_LOOP('',(#10305,#10306,#10307,#10308));
#3038=EDGE_LOOP('',(#10309,#10310,#10311,#10312));
#3039=EDGE_LOOP('',(#10313,#10314,#10315,#10316));
#3040=EDGE_LOOP('',(#10317,#10318,#10319,#10320));
#3041=EDGE_LOOP('',(#10321,#10322,#10323,#10324));
#3042=EDGE_LOOP('',(#10325,#10326,#10327,#10328));
#3043=EDGE_LOOP('',(#10329,#10330,#10331,#10332));
#3044=EDGE_LOOP('',(#10333,#10334,#10335,#10336));
#3045=EDGE_LOOP('',(#10337,#10338,#10339,#10340));
#3046=EDGE_LOOP('',(#10341,#10342,#10343,#10344));
#3047=EDGE_LOOP('',(#10345,#10346,#10347,#10348));
#3048=EDGE_LOOP('',(#10349,#10350,#10351,#10352));
#3049=EDGE_LOOP('',(#10353,#10354,#10355,#10356));
#3050=EDGE_LOOP('',(#10357,#10358,#10359,#10360,#10361,#10362,#10363,#10364,
#10365,#10366,#10367,#10368,#10369,#10370,#10371,#10372,#10373,#10374,#10375,
#10376,#10377,#10378,#10379,#10380,#10381,#10382,#10383,#10384,#10385,#10386,
#10387,#10388,#10389,#10390,#10391,#10392,#10393,#10394,#10395,#10396,#10397,
#10398,#10399,#10400,#10401,#10402,#10403,#10404,#10405,#10406,#10407));
#3051=EDGE_LOOP('',(#10408,#10409,#10410,#10411,#10412));
#3052=EDGE_LOOP('',(#10413,#10414,#10415,#10416));
#3053=EDGE_LOOP('',(#10417,#10418,#10419,#10420,#10421,#10422,#10423,#10424,
#10425,#10426,#10427,#10428,#10429,#10430,#10431,#10432,#10433,#10434,#10435,
#10436,#10437,#10438,#10439,#10440,#10441,#10442,#10443,#10444,#10445,#10446,
#10447,#10448,#10449,#10450,#10451,#10452,#10453,#10454,#10455,#10456,#10457,
#10458,#10459,#10460,#10461,#10462,#10463,#10464,#10465,#10466,#10467,#10468));
#3054=EDGE_LOOP('',(#10469,#10470,#10471));
#3055=EDGE_LOOP('',(#10472,#10473,#10474,#10475));
#3056=EDGE_LOOP('',(#10476,#10477,#10478,#10479));
#3057=EDGE_LOOP('',(#10480,#10481,#10482,#10483));
#3058=EDGE_LOOP('',(#10484,#10485,#10486,#10487));
#3059=EDGE_LOOP('',(#10488,#10489,#10490,#10491));
#3060=EDGE_LOOP('',(#10492,#10493,#10494,#10495));
#3061=EDGE_LOOP('',(#10496,#10497,#10498,#10499,#10500,#10501));
#3062=EDGE_LOOP('',(#10502));
#3063=EDGE_LOOP('',(#10503,#10504,#10505,#10506));
#3064=EDGE_LOOP('',(#10507,#10508,#10509));
#3065=EDGE_LOOP('',(#10510,#10511,#10512,#10513));
#3066=EDGE_LOOP('',(#10514,#10515,#10516));
#3067=EDGE_LOOP('',(#10517,#10518,#10519,#10520));
#3068=EDGE_LOOP('',(#10521,#10522,#10523));
#3069=EDGE_LOOP('',(#10524,#10525,#10526,#10527));
#3070=EDGE_LOOP('',(#10528,#10529,#10530));
#3071=EDGE_LOOP('',(#10531,#10532,#10533,#10534));
#3072=EDGE_LOOP('',(#10535,#10536,#10537));
#3073=EDGE_LOOP('',(#10538,#10539,#10540,#10541));
#3074=EDGE_LOOP('',(#10542,#10543,#10544));
#3075=EDGE_LOOP('',(#10545,#10546,#10547,#10548));
#3076=EDGE_LOOP('',(#10549,#10550,#10551));
#3077=EDGE_LOOP('',(#10552,#10553,#10554,#10555));
#3078=EDGE_LOOP('',(#10556,#10557,#10558));
#3079=EDGE_LOOP('',(#10559,#10560,#10561,#10562));
#3080=EDGE_LOOP('',(#10563,#10564,#10565));
#3081=EDGE_LOOP('',(#10566,#10567,#10568,#10569));
#3082=EDGE_LOOP('',(#10570,#10571,#10572));
#3083=EDGE_LOOP('',(#10573,#10574,#10575,#10576));
#3084=EDGE_LOOP('',(#10577,#10578,#10579));
#3085=EDGE_LOOP('',(#10580,#10581,#10582,#10583));
#3086=EDGE_LOOP('',(#10584,#10585,#10586));
#3087=EDGE_LOOP('',(#10587,#10588,#10589,#10590));
#3088=EDGE_LOOP('',(#10591,#10592,#10593));
#3089=EDGE_LOOP('',(#10594,#10595,#10596,#10597));
#3090=EDGE_LOOP('',(#10598,#10599,#10600));
#3091=EDGE_LOOP('',(#10601,#10602,#10603,#10604));
#3092=EDGE_LOOP('',(#10605,#10606,#10607));
#3093=EDGE_LOOP('',(#10608,#10609,#10610,#10611));
#3094=EDGE_LOOP('',(#10612,#10613,#10614));
#3095=EDGE_LOOP('',(#10615,#10616,#10617,#10618));
#3096=EDGE_LOOP('',(#10619,#10620,#10621,#10622));
#3097=EDGE_LOOP('',(#10623,#10624,#10625,#10626));
#3098=EDGE_LOOP('',(#10627,#10628,#10629,#10630));
#3099=EDGE_LOOP('',(#10631,#10632,#10633,#10634));
#3100=EDGE_LOOP('',(#10635,#10636,#10637));
#3101=EDGE_LOOP('',(#10638,#10639,#10640,#10641));
#3102=EDGE_LOOP('',(#10642,#10643,#10644));
#3103=EDGE_LOOP('',(#10645,#10646,#10647,#10648));
#3104=EDGE_LOOP('',(#10649,#10650,#10651));
#3105=EDGE_LOOP('',(#10652,#10653,#10654,#10655));
#3106=EDGE_LOOP('',(#10656,#10657,#10658));
#3107=EDGE_LOOP('',(#10659,#10660,#10661,#10662));
#3108=EDGE_LOOP('',(#10663,#10664,#10665));
#3109=EDGE_LOOP('',(#10666,#10667,#10668,#10669));
#3110=EDGE_LOOP('',(#10670,#10671,#10672));
#3111=EDGE_LOOP('',(#10673,#10674,#10675,#10676));
#3112=EDGE_LOOP('',(#10677,#10678,#10679));
#3113=EDGE_LOOP('',(#10680,#10681,#10682,#10683));
#3114=EDGE_LOOP('',(#10684,#10685,#10686));
#3115=EDGE_LOOP('',(#10687,#10688,#10689,#10690));
#3116=EDGE_LOOP('',(#10691,#10692,#10693));
#3117=EDGE_LOOP('',(#10694,#10695,#10696,#10697));
#3118=EDGE_LOOP('',(#10698,#10699,#10700));
#3119=EDGE_LOOP('',(#10701,#10702,#10703,#10704));
#3120=EDGE_LOOP('',(#10705,#10706,#10707));
#3121=EDGE_LOOP('',(#10708,#10709,#10710,#10711));
#3122=EDGE_LOOP('',(#10712,#10713,#10714));
#3123=EDGE_LOOP('',(#10715,#10716,#10717,#10718));
#3124=EDGE_LOOP('',(#10719,#10720,#10721));
#3125=EDGE_LOOP('',(#10722,#10723,#10724,#10725));
#3126=EDGE_LOOP('',(#10726,#10727,#10728));
#3127=EDGE_LOOP('',(#10729,#10730,#10731,#10732));
#3128=EDGE_LOOP('',(#10733,#10734,#10735));
#3129=EDGE_LOOP('',(#10736,#10737,#10738,#10739));
#3130=EDGE_LOOP('',(#10740,#10741,#10742));
#3131=EDGE_LOOP('',(#10743,#10744,#10745,#10746));
#3132=EDGE_LOOP('',(#10747,#10748,#10749));
#3133=EDGE_LOOP('',(#10750,#10751,#10752,#10753));
#3134=EDGE_LOOP('',(#10754,#10755,#10756));
#3135=EDGE_LOOP('',(#10757,#10758,#10759,#10760));
#3136=EDGE_LOOP('',(#10761,#10762,#10763));
#3137=EDGE_LOOP('',(#10764,#10765,#10766,#10767));
#3138=EDGE_LOOP('',(#10768,#10769,#10770));
#3139=EDGE_LOOP('',(#10771,#10772,#10773,#10774));
#3140=EDGE_LOOP('',(#10775,#10776,#10777));
#3141=EDGE_LOOP('',(#10778,#10779,#10780,#10781));
#3142=EDGE_LOOP('',(#10782,#10783,#10784));
#3143=EDGE_LOOP('',(#10785,#10786,#10787,#10788));
#3144=EDGE_LOOP('',(#10789,#10790,#10791));
#3145=EDGE_LOOP('',(#10792,#10793,#10794,#10795));
#3146=EDGE_LOOP('',(#10796,#10797,#10798));
#3147=EDGE_LOOP('',(#10799,#10800,#10801,#10802));
#3148=EDGE_LOOP('',(#10803,#10804,#10805));
#3149=EDGE_LOOP('',(#10806,#10807,#10808,#10809));
#3150=EDGE_LOOP('',(#10810,#10811,#10812));
#3151=EDGE_LOOP('',(#10813,#10814,#10815,#10816));
#3152=EDGE_LOOP('',(#10817,#10818,#10819));
#3153=EDGE_LOOP('',(#10820,#10821,#10822,#10823));
#3154=EDGE_LOOP('',(#10824,#10825,#10826));
#3155=EDGE_LOOP('',(#10827,#10828,#10829,#10830));
#3156=EDGE_LOOP('',(#10831,#10832,#10833));
#3157=EDGE_LOOP('',(#10834,#10835,#10836,#10837));
#3158=EDGE_LOOP('',(#10838,#10839,#10840));
#3159=EDGE_LOOP('',(#10841,#10842,#10843,#10844));
#3160=EDGE_LOOP('',(#10845,#10846,#10847));
#3161=EDGE_LOOP('',(#10848,#10849,#10850,#10851));
#3162=EDGE_LOOP('',(#10852,#10853,#10854));
#3163=EDGE_LOOP('',(#10855,#10856,#10857,#10858));
#3164=EDGE_LOOP('',(#10859,#10860,#10861));
#3165=EDGE_LOOP('',(#10862,#10863,#10864,#10865));
#3166=EDGE_LOOP('',(#10866,#10867,#10868));
#3167=EDGE_LOOP('',(#10869,#10870,#10871));
#3168=EDGE_LOOP('',(#10872,#10873,#10874,#10875));
#3169=EDGE_LOOP('',(#10876,#10877,#10878,#10879));
#3170=EDGE_LOOP('',(#10880,#10881,#10882));
#3171=EDGE_LOOP('',(#10883,#10884,#10885,#10886));
#3172=EDGE_LOOP('',(#10887,#10888,#10889));
#3173=EDGE_LOOP('',(#10890,#10891,#10892,#10893));
#3174=EDGE_LOOP('',(#10894,#10895,#10896));
#3175=EDGE_LOOP('',(#10897,#10898,#10899,#10900));
#3176=EDGE_LOOP('',(#10901,#10902,#10903));
#3177=EDGE_LOOP('',(#10904,#10905,#10906,#10907));
#3178=EDGE_LOOP('',(#10908,#10909,#10910));
#3179=EDGE_LOOP('',(#10911,#10912,#10913,#10914));
#3180=EDGE_LOOP('',(#10915,#10916,#10917));
#3181=EDGE_LOOP('',(#10918,#10919,#10920,#10921));
#3182=EDGE_LOOP('',(#10922,#10923,#10924));
#3183=EDGE_LOOP('',(#10925,#10926,#10927,#10928));
#3184=EDGE_LOOP('',(#10929,#10930,#10931));
#3185=EDGE_LOOP('',(#10932,#10933,#10934,#10935));
#3186=EDGE_LOOP('',(#10936,#10937,#10938));
#3187=EDGE_LOOP('',(#10939,#10940,#10941,#10942));
#3188=EDGE_LOOP('',(#10943,#10944,#10945));
#3189=EDGE_LOOP('',(#10946,#10947,#10948,#10949));
#3190=EDGE_LOOP('',(#10950,#10951,#10952));
#3191=EDGE_LOOP('',(#10953,#10954,#10955,#10956));
#3192=EDGE_LOOP('',(#10957,#10958,#10959));
#3193=EDGE_LOOP('',(#10960,#10961,#10962,#10963));
#3194=EDGE_LOOP('',(#10964,#10965,#10966));
#3195=EDGE_LOOP('',(#10967,#10968,#10969,#10970));
#3196=EDGE_LOOP('',(#10971,#10972,#10973));
#3197=EDGE_LOOP('',(#10974,#10975,#10976,#10977));
#3198=EDGE_LOOP('',(#10978,#10979,#10980));
#3199=EDGE_LOOP('',(#10981,#10982,#10983,#10984));
#3200=EDGE_LOOP('',(#10985,#10986,#10987));
#3201=EDGE_LOOP('',(#10988,#10989,#10990,#10991));
#3202=EDGE_LOOP('',(#10992,#10993,#10994));
#3203=EDGE_LOOP('',(#10995,#10996,#10997,#10998));
#3204=EDGE_LOOP('',(#10999,#11000,#11001));
#3205=EDGE_LOOP('',(#11002,#11003,#11004,#11005));
#3206=EDGE_LOOP('',(#11006,#11007,#11008));
#3207=EDGE_LOOP('',(#11009,#11010,#11011,#11012));
#3208=EDGE_LOOP('',(#11013,#11014,#11015,#11016));
#3209=EDGE_LOOP('',(#11017));
#3210=EDGE_LOOP('',(#11018));
#3211=EDGE_LOOP('',(#11019));
#3212=EDGE_LOOP('',(#11020,#11021,#11022,#11023,#11024,#11025));
#3213=EDGE_LOOP('',(#11026,#11027,#11028,#11029));
#3214=EDGE_LOOP('',(#11030));
#3215=EDGE_LOOP('',(#11031,#11032,#11033,#11034,#11035));
#3216=EDGE_LOOP('',(#11036,#11037,#11038,#11039));
#3217=EDGE_LOOP('',(#11040,#11041,#11042,#11043,#11044,#11045,#11046,#11047,
#11048,#11049,#11050,#11051,#11052,#11053,#11054,#11055,#11056,#11057,#11058,
#11059,#11060,#11061,#11062,#11063,#11064,#11065,#11066,#11067,#11068,#11069,
#11070,#11071,#11072,#11073,#11074,#11075,#11076,#11077,#11078,#11079,#11080,
#11081,#11082,#11083,#11084,#11085,#11086,#11087,#11088,#11089,#11090,#11091,
#11092,#11093,#11094,#11095,#11096,#11097,#11098,#11099,#11100,#11101,#11102,
#11103,#11104,#11105,#11106,#11107,#11108,#11109,#11110,#11111,#11112,#11113,
#11114,#11115,#11116,#11117,#11118,#11119,#11120,#11121,#11122,#11123,#11124,
#11125,#11126,#11127,#11128,#11129,#11130,#11131,#11132,#11133,#11134,#11135,
#11136,#11137,#11138,#11139,#11140,#11141,#11142,#11143,#11144,#11145,#11146,
#11147,#11148,#11149,#11150,#11151,#11152,#11153,#11154,#11155,#11156,#11157,
#11158,#11159,#11160,#11161,#11162,#11163,#11164,#11165,#11166,#11167,#11168,
#11169,#11170,#11171,#11172,#11173,#11174,#11175,#11176,#11177,#11178,#11179,
#11180,#11181,#11182,#11183,#11184,#11185,#11186,#11187));
#3218=EDGE_LOOP('',(#11188,#11189,#11190,#11191,#11192,#11193,#11194,#11195,
#11196,#11197,#11198,#11199,#11200,#11201,#11202,#11203,#11204,#11205,#11206,
#11207,#11208,#11209,#11210,#11211,#11212,#11213,#11214,#11215,#11216,#11217,
#11218,#11219,#11220,#11221,#11222,#11223,#11224,#11225,#11226,#11227,#11228,
#11229,#11230,#11231,#11232,#11233,#11234,#11235,#11236,#11237,#11238,#11239,
#11240,#11241,#11242,#11243,#11244,#11245,#11246,#11247,#11248,#11249,#11250,
#11251,#11252,#11253,#11254,#11255,#11256,#11257,#11258,#11259,#11260,#11261,
#11262,#11263));
#3219=EDGE_LOOP('',(#11264));
#3220=EDGE_LOOP('',(#11265,#11266,#11267,#11268,#11269,#11270));
#3221=EDGE_LOOP('',(#11271,#11272,#11273,#11274,#11275));
#3222=EDGE_LOOP('',(#11276));
#3223=EDGE_LOOP('',(#11277));
#3224=EDGE_LOOP('',(#11278,#11279,#11280,#11281,#11282));
#3225=EDGE_LOOP('',(#11283,#11284,#11285,#11286,#11287));
#3226=EDGE_LOOP('',(#11288,#11289,#11290,#11291,#11292,#11293));
#3227=EDGE_LOOP('',(#11294));
#3228=EDGE_LOOP('',(#11295));
#3229=EDGE_LOOP('',(#11296,#11297,#11298,#11299,#11300));
#3230=EDGE_LOOP('',(#11301,#11302,#11303,#11304));
#3231=EDGE_LOOP('',(#11305,#11306,#11307));
#3232=EDGE_LOOP('',(#11308,#11309,#11310));
#3233=EDGE_LOOP('',(#11311,#11312,#11313));
#3234=EDGE_LOOP('',(#11314,#11315,#11316));
#3235=EDGE_LOOP('',(#11317,#11318,#11319));
#3236=EDGE_LOOP('',(#11320,#11321,#11322));
#3237=EDGE_LOOP('',(#11323,#11324,#11325,#11326,#11327,#11328));
#3238=EDGE_LOOP('',(#11329,#11330,#11331,#11332));
#3239=EDGE_LOOP('',(#11333,#11334,#11335,#11336,#11337,#11338));
#3240=EDGE_LOOP('',(#11339,#11340,#11341,#11342,#11343,#11344));
#3241=EDGE_LOOP('',(#11345,#11346,#11347,#11348));
#3242=EDGE_LOOP('',(#11349,#11350,#11351,#11352));
#3243=EDGE_LOOP('',(#11353,#11354,#11355,#11356,#11357,#11358));
#3244=EDGE_LOOP('',(#11359,#11360,#11361,#11362,#11363,#11364,#11365));
#3245=EDGE_LOOP('',(#11366,#11367,#11368,#11369));
#3246=EDGE_LOOP('',(#11370,#11371,#11372,#11373));
#3247=EDGE_LOOP('',(#11374,#11375,#11376,#11377,#11378,#11379));
#3248=EDGE_LOOP('',(#11380,#11381,#11382,#11383));
#3249=EDGE_LOOP('',(#11384,#11385,#11386,#11387));
#3250=EDGE_LOOP('',(#11388,#11389,#11390,#11391));
#3251=EDGE_LOOP('',(#11392,#11393,#11394,#11395));
#3252=EDGE_LOOP('',(#11396,#11397,#11398,#11399,#11400,#11401,#11402,#11403,
#11404,#11405,#11406,#11407,#11408,#11409,#11410,#11411));
#3253=EDGE_LOOP('',(#11412,#11413,#11414));
#3254=EDGE_LOOP('',(#11415,#11416,#11417));
#3255=EDGE_LOOP('',(#11418,#11419,#11420));
#3256=EDGE_LOOP('',(#11421,#11422,#11423));
#3257=EDGE_LOOP('',(#11424,#11425,#11426));
#3258=EDGE_LOOP('',(#11427,#11428,#11429));
#3259=EDGE_LOOP('',(#11430,#11431,#11432,#11433,#11434,#11435,#11436,#11437,
#11438,#11439,#11440,#11441,#11442,#11443,#11444,#11445));
#3260=EDGE_LOOP('',(#11446));
#3261=EDGE_LOOP('',(#11447));
#3262=EDGE_LOOP('',(#11448,#11449,#11450,#11451));
#3263=EDGE_LOOP('',(#11452,#11453,#11454,#11455));
#3264=EDGE_LOOP('',(#11456,#11457,#11458,#11459));
#3265=EDGE_LOOP('',(#11460,#11461,#11462,#11463));
#3266=EDGE_LOOP('',(#11464,#11465,#11466,#11467));
#3267=EDGE_LOOP('',(#11468));
#3268=EDGE_LOOP('',(#11469));
#3269=EDGE_LOOP('',(#11470,#11471,#11472,#11473));
#3270=EDGE_LOOP('',(#11474,#11475,#11476,#11477,#11478));
#3271=EDGE_LOOP('',(#11479,#11480,#11481,#11482));
#3272=LINE('',#16344,#3977);
#3273=LINE('',#16346,#3978);
#3274=LINE('',#16348,#3979);
#3275=LINE('',#16350,#3980);
#3276=LINE('',#16352,#3981);
#3277=LINE('',#16353,#3982);
#3278=LINE('',#16356,#3983);
#3279=LINE('',#16360,#3984);
#3280=LINE('',#16363,#3985);
#3281=LINE('',#16368,#3986);
#3282=LINE('',#16370,#3987);
#3283=LINE('',#16371,#3988);
#3284=LINE('',#16374,#3989);
#3285=LINE('',#16376,#3990);
#3286=LINE('',#16378,#3991);
#3287=LINE('',#16380,#3992);
#3288=LINE('',#16381,#3993);
#3289=LINE('',#16384,#3994);
#3290=LINE('',#16386,#3995);
#3291=LINE('',#16388,#3996);
#3292=LINE('',#16390,#3997);
#3293=LINE('',#16391,#3998);
#3294=LINE('',#16394,#3999);
#3295=LINE('',#16396,#4000);
#3296=LINE('',#16397,#4001);
#3297=LINE('',#16400,#4002);
#3298=LINE('',#16402,#4003);
#3299=LINE('',#16404,#4004);
#3300=LINE('',#16405,#4005);
#3301=LINE('',#16408,#4006);
#3302=LINE('',#16410,#4007);
#3303=LINE('',#16411,#4008);
#3304=LINE('',#16412,#4009);
#3305=LINE('',#16415,#4010);
#3306=LINE('',#16417,#4011);
#3307=LINE('',#16419,#4012);
#3308=LINE('',#16420,#4013);
#3309=LINE('',#16423,#4014);
#3310=LINE('',#16424,#4015);
#3311=LINE('',#16427,#4016);
#3312=LINE('',#16429,#4017);
#3313=LINE('',#16431,#4018);
#3314=LINE('',#16433,#4019);
#3315=LINE('',#16434,#4020);
#3316=LINE('',#16437,#4021);
#3317=LINE('',#16439,#4022);
#3318=LINE('',#16441,#4023);
#3319=LINE('',#16443,#4024);
#3320=LINE('',#16444,#4025);
#3321=LINE('',#16447,#4026);
#3322=LINE('',#16449,#4027);
#3323=LINE('',#16450,#4028);
#3324=LINE('',#16455,#4029);
#3325=LINE('',#16457,#4030);
#3326=LINE('',#16459,#4031);
#3327=LINE('',#16460,#4032);
#3328=LINE('',#16463,#4033);
#3329=LINE('',#16464,#4034);
#3330=LINE('',#16465,#4035);
#3331=LINE('',#16468,#4036);
#3332=LINE('',#16470,#4037);
#3333=LINE('',#16472,#4038);
#3334=LINE('',#16473,#4039);
#3335=LINE('',#16476,#4040);
#3336=LINE('',#16477,#4041);
#3337=LINE('',#16480,#4042);
#3338=LINE('',#16482,#4043);
#3339=LINE('',#16484,#4044);
#3340=LINE('',#16486,#4045);
#3341=LINE('',#16487,#4046);
#3342=LINE('',#16490,#4047);
#3343=LINE('',#16491,#4048);
#3344=LINE('',#16494,#4049);
#3345=LINE('',#16496,#4050);
#3346=LINE('',#16498,#4051);
#3347=LINE('',#16499,#4052);
#3348=LINE('',#16502,#4053);
#3349=LINE('',#16504,#4054);
#3350=LINE('',#16506,#4055);
#3351=LINE('',#16507,#4056);
#3352=LINE('',#16511,#4057);
#3353=LINE('',#16513,#4058);
#3354=LINE('',#16515,#4059);
#3355=LINE('',#16517,#4060);
#3356=LINE('',#16519,#4061);
#3357=LINE('',#16520,#4062);
#3358=LINE('',#16523,#4063);
#3359=LINE('',#16525,#4064);
#3360=LINE('',#16526,#4065);
#3361=LINE('',#16528,#4066);
#3362=LINE('',#16529,#4067);
#3363=LINE('',#16532,#4068);
#3364=LINE('',#16534,#4069);
#3365=LINE('',#16536,#4070);
#3366=LINE('',#16537,#4071);
#3367=LINE('',#16540,#4072);
#3368=LINE('',#16541,#4073);
#3369=LINE('',#16547,#4074);
#3370=LINE('',#16548,#4075);
#3371=LINE('',#16550,#4076);
#3372=LINE('',#16551,#4077);
#3373=LINE('',#16553,#4078);
#3374=LINE('',#16556,#4079);
#3375=LINE('',#16558,#4080);
#3376=LINE('',#16560,#4081);
#3377=LINE('',#16561,#4082);
#3378=LINE('',#16564,#4083);
#3379=LINE('',#16565,#4084);
#3380=LINE('',#16566,#4085);
#3381=LINE('',#16570,#4086);
#3382=LINE('',#16572,#4087);
#3383=LINE('',#16573,#4088);
#3384=LINE('',#16574,#4089);
#3385=LINE('',#16577,#4090);
#3386=LINE('',#16579,#4091);
#3387=LINE('',#16581,#4092);
#3388=LINE('',#16583,#4093);
#3389=LINE('',#16584,#4094);
#3390=LINE('',#16587,#4095);
#3391=LINE('',#16589,#4096);
#3392=LINE('',#16591,#4097);
#3393=LINE('',#16593,#4098);
#3394=LINE('',#16594,#4099);
#3395=LINE('',#16597,#4100);
#3396=LINE('',#16599,#4101);
#3397=LINE('',#16600,#4102);
#3398=LINE('',#16603,#4103);
#3399=LINE('',#16605,#4104);
#3400=LINE('',#16607,#4105);
#3401=LINE('',#16608,#4106);
#3402=LINE('',#16611,#4107);
#3403=LINE('',#16613,#4108);
#3404=LINE('',#16614,#4109);
#3405=LINE('',#16615,#4110);
#3406=LINE('',#16618,#4111);
#3407=LINE('',#16620,#4112);
#3408=LINE('',#16622,#4113);
#3409=LINE('',#16623,#4114);
#3410=LINE('',#16626,#4115);
#3411=LINE('',#16627,#4116);
#3412=LINE('',#16630,#4117);
#3413=LINE('',#16632,#4118);
#3414=LINE('',#16634,#4119);
#3415=LINE('',#16636,#4120);
#3416=LINE('',#16637,#4121);
#3417=LINE('',#16640,#4122);
#3418=LINE('',#16642,#4123);
#3419=LINE('',#16644,#4124);
#3420=LINE('',#16646,#4125);
#3421=LINE('',#16647,#4126);
#3422=LINE('',#16650,#4127);
#3423=LINE('',#16654,#4128);
#3424=LINE('',#16657,#4129);
#3425=LINE('',#16662,#4130);
#3426=LINE('',#16664,#4131);
#3427=LINE('',#16665,#4132);
#3428=LINE('',#16668,#4133);
#3429=LINE('',#16669,#4134);
#3430=LINE('',#16670,#4135);
#3431=LINE('',#16673,#4136);
#3432=LINE('',#16675,#4137);
#3433=LINE('',#16676,#4138);
#3434=LINE('',#16679,#4139);
#3435=LINE('',#16681,#4140);
#3436=LINE('',#16682,#4141);
#3437=LINE('',#16755,#4142);
#3438=LINE('',#16782,#4143);
#3439=LINE('',#16784,#4144);
#3440=LINE('',#16786,#4145);
#3441=LINE('',#16788,#4146);
#3442=LINE('',#16789,#4147);
#3443=LINE('',#16814,#4148);
#3444=LINE('',#16820,#4149);
#3445=LINE('',#16822,#4150);
#3446=LINE('',#16823,#4151);
#3447=LINE('',#16826,#4152);
#3448=LINE('',#16827,#4153);
#3449=LINE('',#16830,#4154);
#3450=LINE('',#16878,#4155);
#3451=LINE('',#16880,#4156);
#3452=LINE('',#16881,#4157);
#3453=LINE('',#16884,#4158);
#3454=LINE('',#16886,#4159);
#3455=LINE('',#16887,#4160);
#3456=LINE('',#16959,#4161);
#3457=LINE('',#16986,#4162);
#3458=LINE('',#16988,#4163);
#3459=LINE('',#16990,#4164);
#3460=LINE('',#16992,#4165);
#3461=LINE('',#16993,#4166);
#3462=LINE('',#17018,#4167);
#3463=LINE('',#17024,#4168);
#3464=LINE('',#17027,#4169);
#3465=LINE('',#17028,#4170);
#3466=LINE('',#17029,#4171);
#3467=LINE('',#17031,#4172);
#3468=LINE('',#17034,#4173);
#3469=LINE('',#17035,#4174);
#3470=LINE('',#17037,#4175);
#3471=LINE('',#17039,#4176);
#3472=LINE('',#17087,#4177);
#3473=LINE('',#17092,#4178);
#3474=LINE('',#17094,#4179);
#3475=LINE('',#17097,#4180);
#3476=LINE('',#17102,#4181);
#3477=LINE('',#17104,#4182);
#3478=LINE('',#17107,#4183);
#3479=LINE('',#17112,#4184);
#3480=LINE('',#17114,#4185);
#3481=LINE('',#17117,#4186);
#3482=LINE('',#17122,#4187);
#3483=LINE('',#17124,#4188);
#3484=LINE('',#17129,#4189);
#3485=LINE('',#17133,#4190);
#3486=LINE('',#17140,#4191);
#3487=LINE('',#17147,#4192);
#3488=LINE('',#17151,#4193);
#3489=LINE('',#17155,#4194);
#3490=LINE('',#17159,#4195);
#3491=LINE('',#17166,#4196);
#3492=LINE('',#17173,#4197);
#3493=LINE('',#17176,#4198);
#3494=LINE('',#17179,#4199);
#3495=LINE('',#17183,#4200);
#3496=LINE('',#17190,#4201);
#3497=LINE('',#17197,#4202);
#3498=LINE('',#17200,#4203);
#3499=LINE('',#17354,#4204);
#3500=LINE('',#17426,#4205);
#3501=LINE('',#17543,#4206);
#3502=LINE('',#17547,#4207);
#3503=LINE('',#17549,#4208);
#3504=LINE('',#17551,#4209);
#3505=LINE('',#17558,#4210);
#3506=LINE('',#17564,#4211);
#3507=LINE('',#18415,#4212);
#3508=LINE('',#18669,#4213);
#3509=LINE('',#18673,#4214);
#3510=LINE('',#21060,#4215);
#3511=LINE('',#21068,#4216);
#3512=LINE('',#21072,#4217);
#3513=LINE('',#21076,#4218);
#3514=LINE('',#21084,#4219);
#3515=LINE('',#21091,#4220);
#3516=LINE('',#21097,#4221);
#3517=LINE('',#21102,#4222);
#3518=LINE('',#21107,#4223);
#3519=LINE('',#21109,#4224);
#3520=LINE('',#21110,#4225);
#3521=LINE('',#21115,#4226);
#3522=LINE('',#21118,#4227);
#3523=LINE('',#21120,#4228);
#3524=LINE('',#21121,#4229);
#3525=LINE('',#21130,#4230);
#3526=LINE('',#21134,#4231);
#3527=LINE('',#21141,#4232);
#3528=LINE('',#21148,#4233);
#3529=LINE('',#21150,#4234);
#3530=LINE('',#21440,#4235);
#3531=LINE('',#21731,#4236);
#3532=LINE('',#21735,#4237);
#3533=LINE('',#21882,#4238);
#3534=LINE('',#24651,#4239);
#3535=LINE('',#24660,#4240);
#3536=LINE('',#24664,#4241);
#3537=LINE('',#24668,#4242);
#3538=LINE('',#24683,#4243);
#3539=LINE('',#24687,#4244);
#3540=LINE('',#24699,#4245);
#3541=LINE('',#24747,#4246);
#3542=LINE('',#24894,#4247);
#3543=LINE('',#25003,#4248);
#3544=LINE('',#25579,#4249);
#3545=LINE('',#25608,#4250);
#3546=LINE('',#25702,#4251);
#3547=LINE('',#25706,#4252);
#3548=LINE('',#25710,#4253);
#3549=LINE('',#25717,#4254);
#3550=LINE('',#25721,#4255);
#3551=LINE('',#25728,#4256);
#3552=LINE('',#25734,#4257);
#3553=LINE('',#25742,#4258);
#3554=LINE('',#25748,#4259);
#3555=LINE('',#25750,#4260);
#3556=LINE('',#25753,#4261);
#3557=LINE('',#25756,#4262);
#3558=LINE('',#25758,#4263);
#3559=LINE('',#25759,#4264);
#3560=LINE('',#25762,#4265);
#3561=LINE('',#25764,#4266);
#3562=LINE('',#25766,#4267);
#3563=LINE('',#25767,#4268);
#3564=LINE('',#25771,#4269);
#3565=LINE('',#25773,#4270);
#3566=LINE('',#25776,#4271);
#3567=LINE('',#25779,#4272);
#3568=LINE('',#25781,#4273);
#3569=LINE('',#25782,#4274);
#3570=LINE('',#25791,#4275);
#3571=LINE('',#25794,#4276);
#3572=LINE('',#25796,#4277);
#3573=LINE('',#25800,#4278);
#3574=LINE('',#25802,#4279);
#3575=LINE('',#25804,#4280);
#3576=LINE('',#25805,#4281);
#3577=LINE('',#25811,#4282);
#3578=LINE('',#25814,#4283);
#3579=LINE('',#25815,#4284);
#3580=LINE('',#25819,#4285);
#3581=LINE('',#25823,#4286);
#3582=LINE('',#25826,#4287);
#3583=LINE('',#25828,#4288);
#3584=LINE('',#25829,#4289);
#3585=LINE('',#25831,#4290);
#3586=LINE('',#25834,#4291);
#3587=LINE('',#25836,#4292);
#3588=LINE('',#25837,#4293);
#3589=LINE('',#25839,#4294);
#3590=LINE('',#25847,#4295);
#3591=LINE('',#25871,#4296);
#3592=LINE('',#25919,#4297);
#3593=LINE('',#25967,#4298);
#3594=LINE('',#26021,#4299);
#3595=LINE('',#26069,#4300);
#3596=LINE('',#26123,#4301);
#3597=LINE('',#26133,#4302);
#3598=LINE('',#26159,#4303);
#3599=LINE('',#26184,#4304);
#3600=LINE('',#26209,#4305);
#3601=LINE('',#26234,#4306);
#3602=LINE('',#26862,#4307);
#3603=LINE('',#26864,#4308);
#3604=LINE('',#26866,#4309);
#3605=LINE('',#26867,#4310);
#3606=LINE('',#26870,#4311);
#3607=LINE('',#26872,#4312);
#3608=LINE('',#26873,#4313);
#3609=LINE('',#26876,#4314);
#3610=LINE('',#26878,#4315);
#3611=LINE('',#26879,#4316);
#3612=LINE('',#26882,#4317);
#3613=LINE('',#26884,#4318);
#3614=LINE('',#26885,#4319);
#3615=LINE('',#26888,#4320);
#3616=LINE('',#26890,#4321);
#3617=LINE('',#26891,#4322);
#3618=LINE('',#26893,#4323);
#3619=LINE('',#26894,#4324);
#3620=LINE('',#26900,#4325);
#3621=LINE('',#26906,#4326);
#3622=LINE('',#26912,#4327);
#3623=LINE('',#26936,#4328);
#3624=LINE('',#26984,#4329);
#3625=LINE('',#27032,#4330);
#3626=LINE('',#27083,#4331);
#3627=LINE('',#27134,#4332);
#3628=LINE('',#27182,#4333);
#3629=LINE('',#27230,#4334);
#3630=LINE('',#27284,#4335);
#3631=LINE('',#27332,#4336);
#3632=LINE('',#27380,#4337);
#3633=LINE('',#27434,#4338);
#3634=LINE('',#27482,#4339);
#3635=LINE('',#27530,#4340);
#3636=LINE('',#27578,#4341);
#3637=LINE('',#27632,#4342);
#3638=LINE('',#27680,#4343);
#3639=LINE('',#27728,#4344);
#3640=LINE('',#27782,#4345);
#3641=LINE('',#27830,#4346);
#3642=LINE('',#27878,#4347);
#3643=LINE('',#27929,#4348);
#3644=LINE('',#27977,#4349);
#3645=LINE('',#28025,#4350);
#3646=LINE('',#28073,#4351);
#3647=LINE('',#28083,#4352);
#3648=LINE('',#28108,#4353);
#3649=LINE('',#28132,#4354);
#3650=LINE('',#28156,#4355);
#3651=LINE('',#28181,#4356);
#3652=LINE('',#28206,#4357);
#3653=LINE('',#28230,#4358);
#3654=LINE('',#28255,#4359);
#3655=LINE('',#28280,#4360);
#3656=LINE('',#28304,#4361);
#3657=LINE('',#28329,#4362);
#3658=LINE('',#28354,#4363);
#3659=LINE('',#28378,#4364);
#3660=LINE('',#28402,#4365);
#3661=LINE('',#28427,#4366);
#3662=LINE('',#28452,#4367);
#3663=LINE('',#28476,#4368);
#3664=LINE('',#28501,#4369);
#3665=LINE('',#28526,#4370);
#3666=LINE('',#28550,#4371);
#3667=LINE('',#28575,#4372);
#3668=LINE('',#28599,#4373);
#3669=LINE('',#28624,#4374);
#3670=LINE('',#30156,#4375);
#3671=LINE('',#30161,#4376);
#3672=LINE('',#30163,#4377);
#3673=LINE('',#30165,#4378);
#3674=LINE('',#30166,#4379);
#3675=LINE('',#30169,#4380);
#3676=LINE('',#30171,#4381);
#3677=LINE('',#30172,#4382);
#3678=LINE('',#30175,#4383);
#3679=LINE('',#30177,#4384);
#3680=LINE('',#30178,#4385);
#3681=LINE('',#30181,#4386);
#3682=LINE('',#30183,#4387);
#3683=LINE('',#30184,#4388);
#3684=LINE('',#30187,#4389);
#3685=LINE('',#30189,#4390);
#3686=LINE('',#30190,#4391);
#3687=LINE('',#30192,#4392);
#3688=LINE('',#30193,#4393);
#3689=LINE('',#30198,#4394);
#3690=LINE('',#30200,#4395);
#3691=LINE('',#30202,#4396);
#3692=LINE('',#30203,#4397);
#3693=LINE('',#30207,#4398);
#3694=LINE('',#30210,#4399);
#3695=LINE('',#30211,#4400);
#3696=LINE('',#30217,#4401);
#3697=LINE('',#30219,#4402);
#3698=LINE('',#30221,#4403);
#3699=LINE('',#30222,#4404);
#3700=LINE('',#30226,#4405);
#3701=LINE('',#30229,#4406);
#3702=LINE('',#30230,#4407);
#3703=LINE('',#30236,#4408);
#3704=LINE('',#30238,#4409);
#3705=LINE('',#30240,#4410);
#3706=LINE('',#30241,#4411);
#3707=LINE('',#30245,#4412);
#3708=LINE('',#30248,#4413);
#3709=LINE('',#30249,#4414);
#3710=LINE('',#30255,#4415);
#3711=LINE('',#30257,#4416);
#3712=LINE('',#30259,#4417);
#3713=LINE('',#30260,#4418);
#3714=LINE('',#30264,#4419);
#3715=LINE('',#30267,#4420);
#3716=LINE('',#30268,#4421);
#3717=LINE('',#30274,#4422);
#3718=LINE('',#30276,#4423);
#3719=LINE('',#30278,#4424);
#3720=LINE('',#30279,#4425);
#3721=LINE('',#30283,#4426);
#3722=LINE('',#30286,#4427);
#3723=LINE('',#30287,#4428);
#3724=LINE('',#30293,#4429);
#3725=LINE('',#30295,#4430);
#3726=LINE('',#30297,#4431);
#3727=LINE('',#30298,#4432);
#3728=LINE('',#30302,#4433);
#3729=LINE('',#30305,#4434);
#3730=LINE('',#30306,#4435);
#3731=LINE('',#30312,#4436);
#3732=LINE('',#30314,#4437);
#3733=LINE('',#30316,#4438);
#3734=LINE('',#30317,#4439);
#3735=LINE('',#30321,#4440);
#3736=LINE('',#30324,#4441);
#3737=LINE('',#30325,#4442);
#3738=LINE('',#30331,#4443);
#3739=LINE('',#30333,#4444);
#3740=LINE('',#30335,#4445);
#3741=LINE('',#30336,#4446);
#3742=LINE('',#30340,#4447);
#3743=LINE('',#30343,#4448);
#3744=LINE('',#30344,#4449);
#3745=LINE('',#30350,#4450);
#3746=LINE('',#30352,#4451);
#3747=LINE('',#30354,#4452);
#3748=LINE('',#30355,#4453);
#3749=LINE('',#30360,#4454);
#3750=LINE('',#30364,#4455);
#3751=LINE('',#30365,#4456);
#3752=LINE('',#30373,#4457);
#3753=LINE('',#30375,#4458);
#3754=LINE('',#30377,#4459);
#3755=LINE('',#30378,#4460);
#3756=LINE('',#30382,#4461);
#3757=LINE('',#30385,#4462);
#3758=LINE('',#30386,#4463);
#3759=LINE('',#30392,#4464);
#3760=LINE('',#30394,#4465);
#3761=LINE('',#30396,#4466);
#3762=LINE('',#30397,#4467);
#3763=LINE('',#30401,#4468);
#3764=LINE('',#30404,#4469);
#3765=LINE('',#30405,#4470);
#3766=LINE('',#30411,#4471);
#3767=LINE('',#30413,#4472);
#3768=LINE('',#30415,#4473);
#3769=LINE('',#30416,#4474);
#3770=LINE('',#30420,#4475);
#3771=LINE('',#30423,#4476);
#3772=LINE('',#30424,#4477);
#3773=LINE('',#30430,#4478);
#3774=LINE('',#30432,#4479);
#3775=LINE('',#30434,#4480);
#3776=LINE('',#30435,#4481);
#3777=LINE('',#30439,#4482);
#3778=LINE('',#30442,#4483);
#3779=LINE('',#30443,#4484);
#3780=LINE('',#30449,#4485);
#3781=LINE('',#30451,#4486);
#3782=LINE('',#30453,#4487);
#3783=LINE('',#30454,#4488);
#3784=LINE('',#30458,#4489);
#3785=LINE('',#30461,#4490);
#3786=LINE('',#30462,#4491);
#3787=LINE('',#30468,#4492);
#3788=LINE('',#30470,#4493);
#3789=LINE('',#30472,#4494);
#3790=LINE('',#30473,#4495);
#3791=LINE('',#30477,#4496);
#3792=LINE('',#30480,#4497);
#3793=LINE('',#30481,#4498);
#3794=LINE('',#30487,#4499);
#3795=LINE('',#30489,#4500);
#3796=LINE('',#30491,#4501);
#3797=LINE('',#30492,#4502);
#3798=LINE('',#30496,#4503);
#3799=LINE('',#30499,#4504);
#3800=LINE('',#30500,#4505);
#3801=LINE('',#30506,#4506);
#3802=LINE('',#30508,#4507);
#3803=LINE('',#30510,#4508);
#3804=LINE('',#30511,#4509);
#3805=LINE('',#30515,#4510);
#3806=LINE('',#30518,#4511);
#3807=LINE('',#30519,#4512);
#3808=LINE('',#30525,#4513);
#3809=LINE('',#30527,#4514);
#3810=LINE('',#30529,#4515);
#3811=LINE('',#30530,#4516);
#3812=LINE('',#30534,#4517);
#3813=LINE('',#30537,#4518);
#3814=LINE('',#30538,#4519);
#3815=LINE('',#30544,#4520);
#3816=LINE('',#30546,#4521);
#3817=LINE('',#30548,#4522);
#3818=LINE('',#30549,#4523);
#3819=LINE('',#30553,#4524);
#3820=LINE('',#30556,#4525);
#3821=LINE('',#30557,#4526);
#3822=LINE('',#30563,#4527);
#3823=LINE('',#30565,#4528);
#3824=LINE('',#30567,#4529);
#3825=LINE('',#30568,#4530);
#3826=LINE('',#30572,#4531);
#3827=LINE('',#30575,#4532);
#3828=LINE('',#30576,#4533);
#3829=LINE('',#30582,#4534);
#3830=LINE('',#30584,#4535);
#3831=LINE('',#30586,#4536);
#3832=LINE('',#30587,#4537);
#3833=LINE('',#30591,#4538);
#3834=LINE('',#30594,#4539);
#3835=LINE('',#30595,#4540);
#3836=LINE('',#30601,#4541);
#3837=LINE('',#30603,#4542);
#3838=LINE('',#30605,#4543);
#3839=LINE('',#30606,#4544);
#3840=LINE('',#30610,#4545);
#3841=LINE('',#30613,#4546);
#3842=LINE('',#30614,#4547);
#3843=LINE('',#30620,#4548);
#3844=LINE('',#30622,#4549);
#3845=LINE('',#30624,#4550);
#3846=LINE('',#30625,#4551);
#3847=LINE('',#30629,#4552);
#3848=LINE('',#30632,#4553);
#3849=LINE('',#30633,#4554);
#3850=LINE('',#30639,#4555);
#3851=LINE('',#30641,#4556);
#3852=LINE('',#30643,#4557);
#3853=LINE('',#30644,#4558);
#3854=LINE('',#30648,#4559);
#3855=LINE('',#30651,#4560);
#3856=LINE('',#30652,#4561);
#3857=LINE('',#30658,#4562);
#3858=LINE('',#30660,#4563);
#3859=LINE('',#30662,#4564);
#3860=LINE('',#30663,#4565);
#3861=LINE('',#30667,#4566);
#3862=LINE('',#30670,#4567);
#3863=LINE('',#30671,#4568);
#3864=LINE('',#30677,#4569);
#3865=LINE('',#30679,#4570);
#3866=LINE('',#30681,#4571);
#3867=LINE('',#30682,#4572);
#3868=LINE('',#30686,#4573);
#3869=LINE('',#30689,#4574);
#3870=LINE('',#30690,#4575);
#3871=LINE('',#30698,#4576);
#3872=LINE('',#30699,#4577);
#3873=LINE('',#30702,#4578);
#3874=LINE('',#30704,#4579);
#3875=LINE('',#30705,#4580);
#3876=LINE('',#30708,#4581);
#3877=LINE('',#30709,#4582);
#3878=LINE('',#30715,#4583);
#3879=LINE('',#30717,#4584);
#3880=LINE('',#30719,#4585);
#3881=LINE('',#30720,#4586);
#3882=LINE('',#30724,#4587);
#3883=LINE('',#30727,#4588);
#3884=LINE('',#30728,#4589);
#3885=LINE('',#30734,#4590);
#3886=LINE('',#30736,#4591);
#3887=LINE('',#30738,#4592);
#3888=LINE('',#30739,#4593);
#3889=LINE('',#30743,#4594);
#3890=LINE('',#30746,#4595);
#3891=LINE('',#30747,#4596);
#3892=LINE('',#30753,#4597);
#3893=LINE('',#30755,#4598);
#3894=LINE('',#30757,#4599);
#3895=LINE('',#30758,#4600);
#3896=LINE('',#30762,#4601);
#3897=LINE('',#30765,#4602);
#3898=LINE('',#30766,#4603);
#3899=LINE('',#30772,#4604);
#3900=LINE('',#30774,#4605);
#3901=LINE('',#30776,#4606);
#3902=LINE('',#30777,#4607);
#3903=LINE('',#30781,#4608);
#3904=LINE('',#30784,#4609);
#3905=LINE('',#30785,#4610);
#3906=LINE('',#30791,#4611);
#3907=LINE('',#30793,#4612);
#3908=LINE('',#30795,#4613);
#3909=LINE('',#30796,#4614);
#3910=LINE('',#30800,#4615);
#3911=LINE('',#30803,#4616);
#3912=LINE('',#30804,#4617);
#3913=LINE('',#30810,#4618);
#3914=LINE('',#30812,#4619);
#3915=LINE('',#30814,#4620);
#3916=LINE('',#30815,#4621);
#3917=LINE('',#30819,#4622);
#3918=LINE('',#30822,#4623);
#3919=LINE('',#30823,#4624);
#3920=LINE('',#30829,#4625);
#3921=LINE('',#30831,#4626);
#3922=LINE('',#30833,#4627);
#3923=LINE('',#30834,#4628);
#3924=LINE('',#30838,#4629);
#3925=LINE('',#30841,#4630);
#3926=LINE('',#30842,#4631);
#3927=LINE('',#30848,#4632);
#3928=LINE('',#30850,#4633);
#3929=LINE('',#30852,#4634);
#3930=LINE('',#30853,#4635);
#3931=LINE('',#30857,#4636);
#3932=LINE('',#30860,#4637);
#3933=LINE('',#30861,#4638);
#3934=LINE('',#30867,#4639);
#3935=LINE('',#30869,#4640);
#3936=LINE('',#30871,#4641);
#3937=LINE('',#30872,#4642);
#3938=LINE('',#30876,#4643);
#3939=LINE('',#30879,#4644);
#3940=LINE('',#30880,#4645);
#3941=LINE('',#30891,#4646);
#3942=LINE('',#30900,#4647);
#3943=LINE('',#30907,#4648);
#3944=LINE('',#30925,#4649);
#3945=LINE('',#30949,#4650);
#3946=LINE('',#30956,#4651);
#3947=LINE('',#30965,#4652);
#3948=LINE('',#30971,#4653);
#3949=LINE('',#30980,#4654);
#3950=LINE('',#30985,#4655);
#3951=LINE('',#30987,#4656);
#3952=LINE('',#30992,#4657);
#3953=LINE('',#31022,#4658);
#3954=LINE('',#31026,#4659);
#3955=LINE('',#31056,#4660);
#3956=LINE('',#31060,#4661);
#3957=LINE('',#31090,#4662);
#3958=LINE('',#31157,#4663);
#3959=LINE('',#31158,#4664);
#3960=LINE('',#31285,#4665);
#3961=LINE('',#31286,#4666);
#3962=LINE('',#31293,#4667);
#3963=LINE('',#31294,#4668);
#3964=LINE('',#31426,#4669);
#3965=LINE('',#31427,#4670);
#3966=LINE('',#31434,#4671);
#3967=LINE('',#31435,#4672);
#3968=LINE('',#31502,#4673);
#3969=LINE('',#31503,#4674);
#3970=LINE('',#31520,#4675);
#3971=LINE('',#31548,#4676);
#3972=LINE('',#31555,#4677);
#3973=LINE('',#31558,#4678);
#3974=LINE('',#31562,#4679);
#3975=LINE('',#31566,#4680);
#3976=LINE('',#31570,#4681);
#3977=VECTOR('',#13626,1.);
#3978=VECTOR('',#13627,1.);
#3979=VECTOR('',#13628,1.);
#3980=VECTOR('',#13629,1.);
#3981=VECTOR('',#13630,1.);
#3982=VECTOR('',#13631,1.);
#3983=VECTOR('',#13634,1.);
#3984=VECTOR('',#13637,1.);
#3985=VECTOR('',#13640,1.);
#3986=VECTOR('',#13645,1.);
#3987=VECTOR('',#13646,1.);
#3988=VECTOR('',#13647,1.);
#3989=VECTOR('',#13650,1.);
#3990=VECTOR('',#13651,1.);
#3991=VECTOR('',#13652,1.);
#3992=VECTOR('',#13653,1.);
#3993=VECTOR('',#13654,1.);
#3994=VECTOR('',#13657,1.);
#3995=VECTOR('',#13658,1.);
#3996=VECTOR('',#13659,1.);
#3997=VECTOR('',#13660,1.);
#3998=VECTOR('',#13661,1.);
#3999=VECTOR('',#13664,1.);
#4000=VECTOR('',#13665,1.);
#4001=VECTOR('',#13666,1.);
#4002=VECTOR('',#13669,1.);
#4003=VECTOR('',#13670,1.);
#4004=VECTOR('',#13671,1.);
#4005=VECTOR('',#13672,1.);
#4006=VECTOR('',#13675,1.);
#4007=VECTOR('',#13676,1.);
#4008=VECTOR('',#13677,1.);
#4009=VECTOR('',#13678,1.);
#4010=VECTOR('',#13681,1.);
#4011=VECTOR('',#13682,1.);
#4012=VECTOR('',#13683,1.);
#4013=VECTOR('',#13684,1.);
#4014=VECTOR('',#13687,1.);
#4015=VECTOR('',#13688,1.);
#4016=VECTOR('',#13691,1.);
#4017=VECTOR('',#13692,1.);
#4018=VECTOR('',#13693,1.);
#4019=VECTOR('',#13694,1.);
#4020=VECTOR('',#13695,1.);
#4021=VECTOR('',#13698,1.);
#4022=VECTOR('',#13699,1.);
#4023=VECTOR('',#13700,1.);
#4024=VECTOR('',#13701,1.);
#4025=VECTOR('',#13702,1.);
#4026=VECTOR('',#13705,1.);
#4027=VECTOR('',#13706,1.);
#4028=VECTOR('',#13707,1.);
#4029=VECTOR('',#13712,1.);
#4030=VECTOR('',#13713,1.);
#4031=VECTOR('',#13714,1.);
#4032=VECTOR('',#13715,1.);
#4033=VECTOR('',#13718,1.);
#4034=VECTOR('',#13719,1.);
#4035=VECTOR('',#13720,1.);
#4036=VECTOR('',#13723,1.);
#4037=VECTOR('',#13724,1.);
#4038=VECTOR('',#13725,1.);
#4039=VECTOR('',#13726,1.);
#4040=VECTOR('',#13729,1.);
#4041=VECTOR('',#13730,1.);
#4042=VECTOR('',#13733,1.);
#4043=VECTOR('',#13734,1.);
#4044=VECTOR('',#13735,1.);
#4045=VECTOR('',#13736,1.);
#4046=VECTOR('',#13737,1.);
#4047=VECTOR('',#13740,1.);
#4048=VECTOR('',#13741,1.);
#4049=VECTOR('',#13744,1.);
#4050=VECTOR('',#13745,1.);
#4051=VECTOR('',#13746,1.);
#4052=VECTOR('',#13747,1.);
#4053=VECTOR('',#13750,1.);
#4054=VECTOR('',#13751,1.);
#4055=VECTOR('',#13752,1.);
#4056=VECTOR('',#13753,1.);
#4057=VECTOR('',#13756,1.);
#4058=VECTOR('',#13757,1.);
#4059=VECTOR('',#13758,1.);
#4060=VECTOR('',#13759,1.);
#4061=VECTOR('',#13760,1.);
#4062=VECTOR('',#13761,1.);
#4063=VECTOR('',#13764,1.);
#4064=VECTOR('',#13765,1.);
#4065=VECTOR('',#13766,1.);
#4066=VECTOR('',#13767,1.);
#4067=VECTOR('',#13768,1.);
#4068=VECTOR('',#13771,1.);
#4069=VECTOR('',#13772,1.);
#4070=VECTOR('',#13773,1.);
#4071=VECTOR('',#13774,1.);
#4072=VECTOR('',#13777,1.);
#4073=VECTOR('',#13778,1.);
#4074=VECTOR('',#13783,1.);
#4075=VECTOR('',#13784,1.);
#4076=VECTOR('',#13785,1.);
#4077=VECTOR('',#13786,1.);
#4078=VECTOR('',#13789,1.);
#4079=VECTOR('',#13792,1.);
#4080=VECTOR('',#13793,1.);
#4081=VECTOR('',#13794,1.);
#4082=VECTOR('',#13795,1.);
#4083=VECTOR('',#13798,1.);
#4084=VECTOR('',#13799,1.);
#4085=VECTOR('',#13800,1.);
#4086=VECTOR('',#13803,1.);
#4087=VECTOR('',#13804,1.);
#4088=VECTOR('',#13805,1.);
#4089=VECTOR('',#13806,1.);
#4090=VECTOR('',#13809,1.);
#4091=VECTOR('',#13810,1.);
#4092=VECTOR('',#13811,1.);
#4093=VECTOR('',#13812,1.);
#4094=VECTOR('',#13813,1.);
#4095=VECTOR('',#13816,1.);
#4096=VECTOR('',#13817,1.);
#4097=VECTOR('',#13818,1.);
#4098=VECTOR('',#13819,1.);
#4099=VECTOR('',#13820,1.);
#4100=VECTOR('',#13823,1.);
#4101=VECTOR('',#13824,1.);
#4102=VECTOR('',#13825,1.);
#4103=VECTOR('',#13828,1.);
#4104=VECTOR('',#13829,1.);
#4105=VECTOR('',#13830,1.);
#4106=VECTOR('',#13831,1.);
#4107=VECTOR('',#13834,1.);
#4108=VECTOR('',#13835,1.);
#4109=VECTOR('',#13836,1.);
#4110=VECTOR('',#13837,1.);
#4111=VECTOR('',#13840,1.);
#4112=VECTOR('',#13841,1.);
#4113=VECTOR('',#13842,1.);
#4114=VECTOR('',#13843,1.);
#4115=VECTOR('',#13846,1.);
#4116=VECTOR('',#13847,1.);
#4117=VECTOR('',#13850,1.);
#4118=VECTOR('',#13851,1.);
#4119=VECTOR('',#13852,1.);
#4120=VECTOR('',#13853,1.);
#4121=VECTOR('',#13854,1.);
#4122=VECTOR('',#13857,1.);
#4123=VECTOR('',#13858,1.);
#4124=VECTOR('',#13859,1.);
#4125=VECTOR('',#13860,1.);
#4126=VECTOR('',#13861,1.);
#4127=VECTOR('',#13864,1.);
#4128=VECTOR('',#13867,1.);
#4129=VECTOR('',#13870,1.);
#4130=VECTOR('',#13875,1.);
#4131=VECTOR('',#13876,1.);
#4132=VECTOR('',#13877,1.);
#4133=VECTOR('',#13880,1.);
#4134=VECTOR('',#13881,1.);
#4135=VECTOR('',#13882,1.);
#4136=VECTOR('',#13885,1.);
#4137=VECTOR('',#13886,1.);
#4138=VECTOR('',#13887,1.);
#4139=VECTOR('',#13890,1.);
#4140=VECTOR('',#13891,1.);
#4141=VECTOR('',#13892,1.);
#4142=VECTOR('',#13895,1.);
#4143=VECTOR('',#13896,1.);
#4144=VECTOR('',#13897,1.);
#4145=VECTOR('',#13898,1.);
#4146=VECTOR('',#13899,1.);
#4147=VECTOR('',#13900,1.);
#4148=VECTOR('',#13909,1.);
#4149=VECTOR('',#13910,1.);
#4150=VECTOR('',#13913,1.);
#4151=VECTOR('',#13914,1.);
#4152=VECTOR('',#13919,1.);
#4153=VECTOR('',#13920,1.);
#4154=VECTOR('',#13925,1.);
#4155=VECTOR('',#13928,1.);
#4156=VECTOR('',#13929,1.);
#4157=VECTOR('',#13930,1.);
#4158=VECTOR('',#13933,1.);
#4159=VECTOR('',#13934,1.);
#4160=VECTOR('',#13935,1.);
#4161=VECTOR('',#13938,1.);
#4162=VECTOR('',#13939,1.);
#4163=VECTOR('',#13940,1.);
#4164=VECTOR('',#13941,1.);
#4165=VECTOR('',#13942,1.);
#4166=VECTOR('',#13943,1.);
#4167=VECTOR('',#13952,1.);
#4168=VECTOR('',#13953,1.);
#4169=VECTOR('',#13956,1.);
#4170=VECTOR('',#13957,1.);
#4171=VECTOR('',#13958,1.);
#4172=VECTOR('',#13961,1.);
#4173=VECTOR('',#13966,1.);
#4174=VECTOR('',#13967,1.);
#4175=VECTOR('',#13970,1.);
#4176=VECTOR('',#13973,1.);
#4177=VECTOR('',#13976,0.36);
#4178=VECTOR('',#13983,0.33);
#4179=VECTOR('',#13986,0.36);
#4180=VECTOR('',#13989,0.36);
#4181=VECTOR('',#13996,0.33);
#4182=VECTOR('',#13999,0.36);
#4183=VECTOR('',#14002,0.36);
#4184=VECTOR('',#14009,0.33);
#4185=VECTOR('',#14012,0.36);
#4186=VECTOR('',#14015,0.36);
#4187=VECTOR('',#14022,0.33);
#4188=VECTOR('',#14025,0.36);
#4189=VECTOR('',#14030,1.35);
#4190=VECTOR('',#14035,1.3);
#4191=VECTOR('',#14044,0.7);
#4192=VECTOR('',#14053,1.3);
#4193=VECTOR('',#14058,1.35);
#4194=VECTOR('',#14063,1.35);
#4195=VECTOR('',#14068,1.3);
#4196=VECTOR('',#14077,0.7);
#4197=VECTOR('',#14086,1.3);
#4198=VECTOR('',#14091,1.35);
#4199=VECTOR('',#14094,1.35);
#4200=VECTOR('',#14099,1.3);
#4201=VECTOR('',#14108,0.7);
#4202=VECTOR('',#14117,1.3);
#4203=VECTOR('',#14122,1.35);
#4204=VECTOR('',#14137,1.);
#4205=VECTOR('',#14138,1.);
#4206=VECTOR('',#14163,1.);
#4207=VECTOR('',#14170,1.);
#4208=VECTOR('',#14173,1.);
#4209=VECTOR('',#14176,1.);
#4210=VECTOR('',#14185,1.39267766952966);
#4211=VECTOR('',#14192,1.63192209588552);
#4212=VECTOR('',#14251,0.205);
#4213=VECTOR('',#14254,0.205);
#4214=VECTOR('',#14259,0.975);
#4215=VECTOR('',#14340,0.980679383410898);
#4216=VECTOR('',#14351,0.521);
#4217=VECTOR('',#14356,0.501);
#4218=VECTOR('',#14361,0.521);
#4219=VECTOR('',#14372,0.12);
#4220=VECTOR('',#14381,0.1);
#4221=VECTOR('',#14388,0.05);
#4222=VECTOR('',#14393,1.);
#4223=VECTOR('',#14398,1.);
#4224=VECTOR('',#14401,1.);
#4225=VECTOR('',#14402,1.);
#4226=VECTOR('',#14407,1.);
#4227=VECTOR('',#14410,1.);
#4228=VECTOR('',#14411,1.);
#4229=VECTOR('',#14412,1.);
#4230=VECTOR('',#14425,0.475);
#4231=VECTOR('',#14430,0.5);
#4232=VECTOR('',#14439,0.48);
#4233=VECTOR('',#14448,0.5);
#4234=VECTOR('',#14451,0.475);
#4235=VECTOR('',#14470,0.205);
#4236=VECTOR('',#14473,0.205);
#4237=VECTOR('',#14478,0.975);
#4238=VECTOR('',#14483,1.63192209588552);
#4239=VECTOR('',#14604,0.980679383410898);
#4240=VECTOR('',#14617,0.521);
#4241=VECTOR('',#14622,0.501);
#4242=VECTOR('',#14627,0.521);
#4243=VECTOR('',#14648,0.76);
#4244=VECTOR('',#14653,1.06);
#4245=VECTOR('',#14668,0.76);
#4246=VECTOR('',#14681,1.06);
#4247=VECTOR('',#14696,1.06);
#4248=VECTOR('',#14723,0.74);
#4249=VECTOR('',#14798,1.06);
#4250=VECTOR('',#14807,0.74);
#4251=VECTOR('',#14830,1.285);
#4252=VECTOR('',#14835,1.3);
#4253=VECTOR('',#14840,1.285);
#4254=VECTOR('',#14849,0.5);
#4255=VECTOR('',#14854,0.515);
#4256=VECTOR('',#14865,0.515);
#4257=VECTOR('',#14872,0.5);
#4258=VECTOR('',#14883,0.8);
#4259=VECTOR('',#14890,1.);
#4260=VECTOR('',#14891,1.);
#4261=VECTOR('',#14894,1.);
#4262=VECTOR('',#14897,1.);
#4263=VECTOR('',#14898,1.);
#4264=VECTOR('',#14899,1.);
#4265=VECTOR('',#14902,1.);
#4266=VECTOR('',#14903,1.);
#4267=VECTOR('',#14904,1.);
#4268=VECTOR('',#14905,1.);
#4269=VECTOR('',#14908,1.);
#4270=VECTOR('',#14909,1.);
#4271=VECTOR('',#14912,1.);
#4272=VECTOR('',#14915,1.);
#4273=VECTOR('',#14916,1.);
#4274=VECTOR('',#14917,1.);
#4275=VECTOR('',#14930,1.);
#4276=VECTOR('',#14933,1.);
#4277=VECTOR('',#14934,1.);
#4278=VECTOR('',#14937,1.);
#4279=VECTOR('',#14938,1.);
#4280=VECTOR('',#14939,1.);
#4281=VECTOR('',#14940,1.);
#4282=VECTOR('',#14947,1.);
#4283=VECTOR('',#14950,1.);
#4284=VECTOR('',#14951,1.);
#4285=VECTOR('',#14956,0.05);
#4286=VECTOR('',#14961,0.05);
#4287=VECTOR('',#14964,1.);
#4288=VECTOR('',#14965,1.);
#4289=VECTOR('',#14966,1.);
#4290=VECTOR('',#14969,1.);
#4291=VECTOR('',#14972,1.);
#4292=VECTOR('',#14973,1.);
#4293=VECTOR('',#14974,1.);
#4294=VECTOR('',#14977,1.);
#4295=VECTOR('',#14988,0.2);
#4296=VECTOR('',#14993,0.2);
#4297=VECTOR('',#14996,0.2);
#4298=VECTOR('',#14999,0.2);
#4299=VECTOR('',#15002,0.2);
#4300=VECTOR('',#15005,0.2);
#4301=VECTOR('',#15008,0.15555);
#4302=VECTOR('',#15013,0.15555);
#4303=VECTOR('',#15018,0.15555);
#4304=VECTOR('',#15021,0.15555);
#4305=VECTOR('',#15024,0.15555);
#4306=VECTOR('',#15027,0.15555);
#4307=VECTOR('',#15046,1.);
#4308=VECTOR('',#15047,1.);
#4309=VECTOR('',#15048,1.);
#4310=VECTOR('',#15049,1.);
#4311=VECTOR('',#15052,1.);
#4312=VECTOR('',#15053,1.);
#4313=VECTOR('',#15054,1.);
#4314=VECTOR('',#15057,1.);
#4315=VECTOR('',#15058,1.);
#4316=VECTOR('',#15059,1.);
#4317=VECTOR('',#15062,1.);
#4318=VECTOR('',#15063,1.);
#4319=VECTOR('',#15064,1.);
#4320=VECTOR('',#15067,1.);
#4321=VECTOR('',#15068,1.);
#4322=VECTOR('',#15069,1.);
#4323=VECTOR('',#15072,1.);
#4324=VECTOR('',#15073,1.);
#4325=VECTOR('',#15082,0.185);
#4326=VECTOR('',#15091,0.1625);
#4327=VECTOR('',#15098,0.3);
#4328=VECTOR('',#15103,0.3);
#4329=VECTOR('',#15106,0.3);
#4330=VECTOR('',#15109,0.3);
#4331=VECTOR('',#15112,0.3);
#4332=VECTOR('',#15115,0.3);
#4333=VECTOR('',#15118,0.3);
#4334=VECTOR('',#15121,0.3);
#4335=VECTOR('',#15124,0.3);
#4336=VECTOR('',#15127,0.3);
#4337=VECTOR('',#15130,0.3);
#4338=VECTOR('',#15133,0.3);
#4339=VECTOR('',#15136,0.3);
#4340=VECTOR('',#15139,0.3);
#4341=VECTOR('',#15142,0.3);
#4342=VECTOR('',#15145,0.3);
#4343=VECTOR('',#15148,0.3);
#4344=VECTOR('',#15151,0.3);
#4345=VECTOR('',#15154,0.3);
#4346=VECTOR('',#15157,0.3);
#4347=VECTOR('',#15160,0.3);
#4348=VECTOR('',#15163,0.3);
#4349=VECTOR('',#15166,0.3);
#4350=VECTOR('',#15169,0.3);
#4351=VECTOR('',#15172,0.237175);
#4352=VECTOR('',#15177,0.237175);
#4353=VECTOR('',#15182,0.237175);
#4354=VECTOR('',#15185,0.237175);
#4355=VECTOR('',#15188,0.237175);
#4356=VECTOR('',#15191,0.237175);
#4357=VECTOR('',#15194,0.237175);
#4358=VECTOR('',#15197,0.237175);
#4359=VECTOR('',#15200,0.237175);
#4360=VECTOR('',#15203,0.237175);
#4361=VECTOR('',#15206,0.237175);
#4362=VECTOR('',#15209,0.237175);
#4363=VECTOR('',#15212,0.237175);
#4364=VECTOR('',#15215,0.237175);
#4365=VECTOR('',#15218,0.237175);
#4366=VECTOR('',#15221,0.237175);
#4367=VECTOR('',#15224,0.237175);
#4368=VECTOR('',#15227,0.237175);
#4369=VECTOR('',#15230,0.237175);
#4370=VECTOR('',#15233,0.237175);
#4371=VECTOR('',#15236,0.237175);
#4372=VECTOR('',#15239,0.237175);
#4373=VECTOR('',#15242,0.237175);
#4374=VECTOR('',#15245,0.237175);
#4375=VECTOR('',#15258,0.124996333279554);
#4376=VECTOR('',#15263,1.);
#4377=VECTOR('',#15264,1.);
#4378=VECTOR('',#15265,1.);
#4379=VECTOR('',#15266,1.);
#4380=VECTOR('',#15269,1.);
#4381=VECTOR('',#15270,1.);
#4382=VECTOR('',#15271,1.);
#4383=VECTOR('',#15274,1.);
#4384=VECTOR('',#15275,1.);
#4385=VECTOR('',#15276,1.);
#4386=VECTOR('',#15279,1.);
#4387=VECTOR('',#15280,1.);
#4388=VECTOR('',#15281,1.);
#4389=VECTOR('',#15284,1.);
#4390=VECTOR('',#15285,1.);
#4391=VECTOR('',#15286,1.);
#4392=VECTOR('',#15289,1.);
#4393=VECTOR('',#15290,1.);
#4394=VECTOR('',#15295,1.);
#4395=VECTOR('',#15296,1.);
#4396=VECTOR('',#15297,1.);
#4397=VECTOR('',#15298,1.);
#4398=VECTOR('',#15303,1.);
#4399=VECTOR('',#15306,1.);
#4400=VECTOR('',#15307,1.);
#4401=VECTOR('',#15314,1.);
#4402=VECTOR('',#15315,1.);
#4403=VECTOR('',#15316,1.);
#4404=VECTOR('',#15317,1.);
#4405=VECTOR('',#15322,1.);
#4406=VECTOR('',#15325,1.);
#4407=VECTOR('',#15326,1.);
#4408=VECTOR('',#15333,1.);
#4409=VECTOR('',#15334,1.);
#4410=VECTOR('',#15335,1.);
#4411=VECTOR('',#15336,1.);
#4412=VECTOR('',#15341,1.);
#4413=VECTOR('',#15344,1.);
#4414=VECTOR('',#15345,1.);
#4415=VECTOR('',#15352,1.);
#4416=VECTOR('',#15353,1.);
#4417=VECTOR('',#15354,1.);
#4418=VECTOR('',#15355,1.);
#4419=VECTOR('',#15360,1.);
#4420=VECTOR('',#15363,1.);
#4421=VECTOR('',#15364,1.);
#4422=VECTOR('',#15371,1.);
#4423=VECTOR('',#15372,1.);
#4424=VECTOR('',#15373,1.);
#4425=VECTOR('',#15374,1.);
#4426=VECTOR('',#15379,1.);
#4427=VECTOR('',#15382,1.);
#4428=VECTOR('',#15383,1.);
#4429=VECTOR('',#15390,1.);
#4430=VECTOR('',#15391,1.);
#4431=VECTOR('',#15392,1.);
#4432=VECTOR('',#15393,1.);
#4433=VECTOR('',#15398,1.);
#4434=VECTOR('',#15401,1.);
#4435=VECTOR('',#15402,1.);
#4436=VECTOR('',#15409,1.);
#4437=VECTOR('',#15410,1.);
#4438=VECTOR('',#15411,1.);
#4439=VECTOR('',#15412,1.);
#4440=VECTOR('',#15417,1.);
#4441=VECTOR('',#15420,1.);
#4442=VECTOR('',#15421,1.);
#4443=VECTOR('',#15428,1.);
#4444=VECTOR('',#15429,1.);
#4445=VECTOR('',#15430,1.);
#4446=VECTOR('',#15431,1.);
#4447=VECTOR('',#15436,1.);
#4448=VECTOR('',#15439,1.);
#4449=VECTOR('',#15440,1.);
#4450=VECTOR('',#15447,1.);
#4451=VECTOR('',#15448,1.);
#4452=VECTOR('',#15449,1.);
#4453=VECTOR('',#15450,1.);
#4454=VECTOR('',#15455,1.);
#4455=VECTOR('',#15460,1.);
#4456=VECTOR('',#15461,1.);
#4457=VECTOR('',#15470,1.);
#4458=VECTOR('',#15471,1.);
#4459=VECTOR('',#15472,1.);
#4460=VECTOR('',#15473,1.);
#4461=VECTOR('',#15478,1.);
#4462=VECTOR('',#15481,1.);
#4463=VECTOR('',#15482,1.);
#4464=VECTOR('',#15489,1.);
#4465=VECTOR('',#15490,1.);
#4466=VECTOR('',#15491,1.);
#4467=VECTOR('',#15492,1.);
#4468=VECTOR('',#15497,1.);
#4469=VECTOR('',#15500,1.);
#4470=VECTOR('',#15501,1.);
#4471=VECTOR('',#15508,1.);
#4472=VECTOR('',#15509,1.);
#4473=VECTOR('',#15510,1.);
#4474=VECTOR('',#15511,1.);
#4475=VECTOR('',#15516,1.);
#4476=VECTOR('',#15519,1.);
#4477=VECTOR('',#15520,1.);
#4478=VECTOR('',#15527,1.);
#4479=VECTOR('',#15528,1.);
#4480=VECTOR('',#15529,1.);
#4481=VECTOR('',#15530,1.);
#4482=VECTOR('',#15535,1.);
#4483=VECTOR('',#15538,1.);
#4484=VECTOR('',#15539,1.);
#4485=VECTOR('',#15546,1.);
#4486=VECTOR('',#15547,1.);
#4487=VECTOR('',#15548,1.);
#4488=VECTOR('',#15549,1.);
#4489=VECTOR('',#15554,1.);
#4490=VECTOR('',#15557,1.);
#4491=VECTOR('',#15558,1.);
#4492=VECTOR('',#15565,1.);
#4493=VECTOR('',#15566,1.);
#4494=VECTOR('',#15567,1.);
#4495=VECTOR('',#15568,1.);
#4496=VECTOR('',#15573,1.);
#4497=VECTOR('',#15576,1.);
#4498=VECTOR('',#15577,1.);
#4499=VECTOR('',#15584,1.);
#4500=VECTOR('',#15585,1.);
#4501=VECTOR('',#15586,1.);
#4502=VECTOR('',#15587,1.);
#4503=VECTOR('',#15592,1.);
#4504=VECTOR('',#15595,1.);
#4505=VECTOR('',#15596,1.);
#4506=VECTOR('',#15603,1.);
#4507=VECTOR('',#15604,1.);
#4508=VECTOR('',#15605,1.);
#4509=VECTOR('',#15606,1.);
#4510=VECTOR('',#15611,1.);
#4511=VECTOR('',#15614,1.);
#4512=VECTOR('',#15615,1.);
#4513=VECTOR('',#15622,1.);
#4514=VECTOR('',#15623,1.);
#4515=VECTOR('',#15624,1.);
#4516=VECTOR('',#15625,1.);
#4517=VECTOR('',#15630,1.);
#4518=VECTOR('',#15633,1.);
#4519=VECTOR('',#15634,1.);
#4520=VECTOR('',#15641,1.);
#4521=VECTOR('',#15642,1.);
#4522=VECTOR('',#15643,1.);
#4523=VECTOR('',#15644,1.);
#4524=VECTOR('',#15649,1.);
#4525=VECTOR('',#15652,1.);
#4526=VECTOR('',#15653,1.);
#4527=VECTOR('',#15660,1.);
#4528=VECTOR('',#15661,1.);
#4529=VECTOR('',#15662,1.);
#4530=VECTOR('',#15663,1.);
#4531=VECTOR('',#15668,1.);
#4532=VECTOR('',#15671,1.);
#4533=VECTOR('',#15672,1.);
#4534=VECTOR('',#15679,1.);
#4535=VECTOR('',#15680,1.);
#4536=VECTOR('',#15681,1.);
#4537=VECTOR('',#15682,1.);
#4538=VECTOR('',#15687,1.);
#4539=VECTOR('',#15690,1.);
#4540=VECTOR('',#15691,1.);
#4541=VECTOR('',#15698,1.);
#4542=VECTOR('',#15699,1.);
#4543=VECTOR('',#15700,1.);
#4544=VECTOR('',#15701,1.);
#4545=VECTOR('',#15706,1.);
#4546=VECTOR('',#15709,1.);
#4547=VECTOR('',#15710,1.);
#4548=VECTOR('',#15717,1.);
#4549=VECTOR('',#15718,1.);
#4550=VECTOR('',#15719,1.);
#4551=VECTOR('',#15720,1.);
#4552=VECTOR('',#15725,1.);
#4553=VECTOR('',#15728,1.);
#4554=VECTOR('',#15729,1.);
#4555=VECTOR('',#15736,1.);
#4556=VECTOR('',#15737,1.);
#4557=VECTOR('',#15738,1.);
#4558=VECTOR('',#15739,1.);
#4559=VECTOR('',#15744,1.);
#4560=VECTOR('',#15747,1.);
#4561=VECTOR('',#15748,1.);
#4562=VECTOR('',#15755,1.);
#4563=VECTOR('',#15756,1.);
#4564=VECTOR('',#15757,1.);
#4565=VECTOR('',#15758,1.);
#4566=VECTOR('',#15763,1.);
#4567=VECTOR('',#15766,1.);
#4568=VECTOR('',#15767,1.);
#4569=VECTOR('',#15774,1.);
#4570=VECTOR('',#15775,1.);
#4571=VECTOR('',#15776,1.);
#4572=VECTOR('',#15777,1.);
#4573=VECTOR('',#15782,1.);
#4574=VECTOR('',#15785,1.);
#4575=VECTOR('',#15786,1.);
#4576=VECTOR('',#15795,1.);
#4577=VECTOR('',#15796,1.);
#4578=VECTOR('',#15799,1.);
#4579=VECTOR('',#15800,1.);
#4580=VECTOR('',#15801,1.);
#4581=VECTOR('',#15804,1.);
#4582=VECTOR('',#15805,1.);
#4583=VECTOR('',#15812,1.);
#4584=VECTOR('',#15813,1.);
#4585=VECTOR('',#15814,1.);
#4586=VECTOR('',#15815,1.);
#4587=VECTOR('',#15820,1.);
#4588=VECTOR('',#15823,1.);
#4589=VECTOR('',#15824,1.);
#4590=VECTOR('',#15831,1.);
#4591=VECTOR('',#15832,1.);
#4592=VECTOR('',#15833,1.);
#4593=VECTOR('',#15834,1.);
#4594=VECTOR('',#15839,1.);
#4595=VECTOR('',#15842,1.);
#4596=VECTOR('',#15843,1.);
#4597=VECTOR('',#15850,1.);
#4598=VECTOR('',#15851,1.);
#4599=VECTOR('',#15852,1.);
#4600=VECTOR('',#15853,1.);
#4601=VECTOR('',#15858,1.);
#4602=VECTOR('',#15861,1.);
#4603=VECTOR('',#15862,1.);
#4604=VECTOR('',#15869,1.);
#4605=VECTOR('',#15870,1.);
#4606=VECTOR('',#15871,1.);
#4607=VECTOR('',#15872,1.);
#4608=VECTOR('',#15877,1.);
#4609=VECTOR('',#15880,1.);
#4610=VECTOR('',#15881,1.);
#4611=VECTOR('',#15888,1.);
#4612=VECTOR('',#15889,1.);
#4613=VECTOR('',#15890,1.);
#4614=VECTOR('',#15891,1.);
#4615=VECTOR('',#15896,1.);
#4616=VECTOR('',#15899,1.);
#4617=VECTOR('',#15900,1.);
#4618=VECTOR('',#15907,1.);
#4619=VECTOR('',#15908,1.);
#4620=VECTOR('',#15909,1.);
#4621=VECTOR('',#15910,1.);
#4622=VECTOR('',#15915,1.);
#4623=VECTOR('',#15918,1.);
#4624=VECTOR('',#15919,1.);
#4625=VECTOR('',#15926,1.);
#4626=VECTOR('',#15927,1.);
#4627=VECTOR('',#15928,1.);
#4628=VECTOR('',#15929,1.);
#4629=VECTOR('',#15934,1.);
#4630=VECTOR('',#15937,1.);
#4631=VECTOR('',#15938,1.);
#4632=VECTOR('',#15945,1.);
#4633=VECTOR('',#15946,1.);
#4634=VECTOR('',#15947,1.);
#4635=VECTOR('',#15948,1.);
#4636=VECTOR('',#15953,1.);
#4637=VECTOR('',#15956,1.);
#4638=VECTOR('',#15957,1.);
#4639=VECTOR('',#15964,1.);
#4640=VECTOR('',#15965,1.);
#4641=VECTOR('',#15966,1.);
#4642=VECTOR('',#15967,1.);
#4643=VECTOR('',#15972,1.);
#4644=VECTOR('',#15975,1.);
#4645=VECTOR('',#15976,1.);
#4646=VECTOR('',#15991,0.298);
#4647=VECTOR('',#16004,0.28);
#4648=VECTOR('',#16015,0.49);
#4649=VECTOR('',#16050,0.5);
#4650=VECTOR('',#16095,0.48);
#4651=VECTOR('',#16104,0.59);
#4652=VECTOR('',#16115,0.6);
#4653=VECTOR('',#16122,0.33);
#4654=VECTOR('',#16133,0.32);
#4655=VECTOR('',#16140,0.33);
#4656=VECTOR('',#16143,0.59);
#4657=VECTOR('',#16148,1.);
#4658=VECTOR('',#16151,1.);
#4659=VECTOR('',#16154,1.);
#4660=VECTOR('',#16157,1.);
#4661=VECTOR('',#16160,1.);
#4662=VECTOR('',#16163,1.);
#4663=VECTOR('',#16166,1.);
#4664=VECTOR('',#16167,1.);
#4665=VECTOR('',#16170,1.);
#4666=VECTOR('',#16171,1.);
#4667=VECTOR('',#16174,1.);
#4668=VECTOR('',#16175,1.);
#4669=VECTOR('',#16178,1.);
#4670=VECTOR('',#16179,1.);
#4671=VECTOR('',#16182,1.);
#4672=VECTOR('',#16183,1.);
#4673=VECTOR('',#16186,1.);
#4674=VECTOR('',#16187,1.);
#4675=VECTOR('',#16198,0.551175134594813);
#4676=VECTOR('',#16227,0.473593266739737);
#4677=VECTOR('',#16236,0.348075378797541);
#4678=VECTOR('',#16239,0.325);
#4679=VECTOR('',#16244,0.312424621202459);
#4680=VECTOR('',#16249,0.305);
#4681=VECTOR('',#16254,0.325);
#4682=VERTEX_POINT('',#16342);
#4683=VERTEX_POINT('',#16343);
#4684=VERTEX_POINT('',#16345);
#4685=VERTEX_POINT('',#16347);
#4686=VERTEX_POINT('',#16349);
#4687=VERTEX_POINT('',#16351);
#4688=VERTEX_POINT('',#16355);
#4689=VERTEX_POINT('',#16357);
#4690=VERTEX_POINT('',#16359);
#4691=VERTEX_POINT('',#16361);
#4692=VERTEX_POINT('',#16364);
#4693=VERTEX_POINT('',#16367);
#4694=VERTEX_POINT('',#16369);
#4695=VERTEX_POINT('',#16373);
#4696=VERTEX_POINT('',#16375);
#4697=VERTEX_POINT('',#16377);
#4698=VERTEX_POINT('',#16379);
#4699=VERTEX_POINT('',#16383);
#4700=VERTEX_POINT('',#16385);
#4701=VERTEX_POINT('',#16387);
#4702=VERTEX_POINT('',#16389);
#4703=VERTEX_POINT('',#16393);
#4704=VERTEX_POINT('',#16395);
#4705=VERTEX_POINT('',#16399);
#4706=VERTEX_POINT('',#16401);
#4707=VERTEX_POINT('',#16403);
#4708=VERTEX_POINT('',#16407);
#4709=VERTEX_POINT('',#16409);
#4710=VERTEX_POINT('',#16414);
#4711=VERTEX_POINT('',#16416);
#4712=VERTEX_POINT('',#16418);
#4713=VERTEX_POINT('',#16422);
#4714=VERTEX_POINT('',#16426);
#4715=VERTEX_POINT('',#16428);
#4716=VERTEX_POINT('',#16430);
#4717=VERTEX_POINT('',#16432);
#4718=VERTEX_POINT('',#16436);
#4719=VERTEX_POINT('',#16438);
#4720=VERTEX_POINT('',#16440);
#4721=VERTEX_POINT('',#16442);
#4722=VERTEX_POINT('',#16446);
#4723=VERTEX_POINT('',#16448);
#4724=VERTEX_POINT('',#16451);
#4725=VERTEX_POINT('',#16454);
#4726=VERTEX_POINT('',#16456);
#4727=VERTEX_POINT('',#16458);
#4728=VERTEX_POINT('',#16462);
#4729=VERTEX_POINT('',#16467);
#4730=VERTEX_POINT('',#16469);
#4731=VERTEX_POINT('',#16471);
#4732=VERTEX_POINT('',#16475);
#4733=VERTEX_POINT('',#16479);
#4734=VERTEX_POINT('',#16481);
#4735=VERTEX_POINT('',#16483);
#4736=VERTEX_POINT('',#16485);
#4737=VERTEX_POINT('',#16489);
#4738=VERTEX_POINT('',#16493);
#4739=VERTEX_POINT('',#16495);
#4740=VERTEX_POINT('',#16497);
#4741=VERTEX_POINT('',#16501);
#4742=VERTEX_POINT('',#16503);
#4743=VERTEX_POINT('',#16505);
#4744=VERTEX_POINT('',#16509);
#4745=VERTEX_POINT('',#16510);
#4746=VERTEX_POINT('',#16512);
#4747=VERTEX_POINT('',#16514);
#4748=VERTEX_POINT('',#16516);
#4749=VERTEX_POINT('',#16518);
#4750=VERTEX_POINT('',#16522);
#4751=VERTEX_POINT('',#16524);
#4752=VERTEX_POINT('',#16527);
#4753=VERTEX_POINT('',#16531);
#4754=VERTEX_POINT('',#16533);
#4755=VERTEX_POINT('',#16535);
#4756=VERTEX_POINT('',#16539);
#4757=VERTEX_POINT('',#16542);
#4758=VERTEX_POINT('',#16545);
#4759=VERTEX_POINT('',#16546);
#4760=VERTEX_POINT('',#16549);
#4761=VERTEX_POINT('',#16555);
#4762=VERTEX_POINT('',#16557);
#4763=VERTEX_POINT('',#16559);
#4764=VERTEX_POINT('',#16563);
#4765=VERTEX_POINT('',#16568);
#4766=VERTEX_POINT('',#16569);
#4767=VERTEX_POINT('',#16571);
#4768=VERTEX_POINT('',#16576);
#4769=VERTEX_POINT('',#16578);
#4770=VERTEX_POINT('',#16580);
#4771=VERTEX_POINT('',#16582);
#4772=VERTEX_POINT('',#16586);
#4773=VERTEX_POINT('',#16588);
#4774=VERTEX_POINT('',#16590);
#4775=VERTEX_POINT('',#16592);
#4776=VERTEX_POINT('',#16596);
#4777=VERTEX_POINT('',#16598);
#4778=VERTEX_POINT('',#16602);
#4779=VERTEX_POINT('',#16604);
#4780=VERTEX_POINT('',#16606);
#4781=VERTEX_POINT('',#16610);
#4782=VERTEX_POINT('',#16612);
#4783=VERTEX_POINT('',#16617);
#4784=VERTEX_POINT('',#16619);
#4785=VERTEX_POINT('',#16621);
#4786=VERTEX_POINT('',#16625);
#4787=VERTEX_POINT('',#16629);
#4788=VERTEX_POINT('',#16631);
#4789=VERTEX_POINT('',#16633);
#4790=VERTEX_POINT('',#16635);
#4791=VERTEX_POINT('',#16639);
#4792=VERTEX_POINT('',#16641);
#4793=VERTEX_POINT('',#16643);
#4794=VERTEX_POINT('',#16645);
#4795=VERTEX_POINT('',#16649);
#4796=VERTEX_POINT('',#16651);
#4797=VERTEX_POINT('',#16653);
#4798=VERTEX_POINT('',#16655);
#4799=VERTEX_POINT('',#16658);
#4800=VERTEX_POINT('',#16661);
#4801=VERTEX_POINT('',#16663);
#4802=VERTEX_POINT('',#16667);
#4803=VERTEX_POINT('',#16672);
#4804=VERTEX_POINT('',#16674);
#4805=VERTEX_POINT('',#16678);
#4806=VERTEX_POINT('',#16680);
#4807=VERTEX_POINT('',#16699);
#4808=VERTEX_POINT('',#16700);
#4809=VERTEX_POINT('',#16729);
#4810=VERTEX_POINT('',#16739);
#4811=VERTEX_POINT('',#16749);
#4812=VERTEX_POINT('',#16754);
#4813=VERTEX_POINT('',#16756);
#4814=VERTEX_POINT('',#16761);
#4815=VERTEX_POINT('',#16771);
#4816=VERTEX_POINT('',#16776);
#4817=VERTEX_POINT('',#16781);
#4818=VERTEX_POINT('',#16783);
#4819=VERTEX_POINT('',#16785);
#4820=VERTEX_POINT('',#16787);
#4821=VERTEX_POINT('',#16790);
#4822=VERTEX_POINT('',#16792);
#4823=VERTEX_POINT('',#16794);
#4824=VERTEX_POINT('',#16796);
#4825=VERTEX_POINT('',#16815);
#4826=VERTEX_POINT('',#16847);
#4827=VERTEX_POINT('',#16877);
#4828=VERTEX_POINT('',#16879);
#4829=VERTEX_POINT('',#16883);
#4830=VERTEX_POINT('',#16885);
#4831=VERTEX_POINT('',#16904);
#4832=VERTEX_POINT('',#16905);
#4833=VERTEX_POINT('',#16934);
#4834=VERTEX_POINT('',#16944);
#4835=VERTEX_POINT('',#16953);
#4836=VERTEX_POINT('',#16958);
#4837=VERTEX_POINT('',#16960);
#4838=VERTEX_POINT('',#16965);
#4839=VERTEX_POINT('',#16975);
#4840=VERTEX_POINT('',#16980);
#4841=VERTEX_POINT('',#16985);
#4842=VERTEX_POINT('',#16987);
#4843=VERTEX_POINT('',#16989);
#4844=VERTEX_POINT('',#16991);
#4845=VERTEX_POINT('',#16994);
#4846=VERTEX_POINT('',#16996);
#4847=VERTEX_POINT('',#16998);
#4848=VERTEX_POINT('',#17000);
#4849=VERTEX_POINT('',#17019);
#4850=VERTEX_POINT('',#17026);
#4851=VERTEX_POINT('',#17056);
#4852=VERTEX_POINT('',#17086);
#4853=VERTEX_POINT('',#17090);
#4854=VERTEX_POINT('',#17096);
#4855=VERTEX_POINT('',#17100);
#4856=VERTEX_POINT('',#17106);
#4857=VERTEX_POINT('',#17110);
#4858=VERTEX_POINT('',#17116);
#4859=VERTEX_POINT('',#17120);
#4860=VERTEX_POINT('',#17126);
#4861=VERTEX_POINT('',#17128);
#4862=VERTEX_POINT('',#17132);
#4863=VERTEX_POINT('',#17136);
#4864=VERTEX_POINT('',#17139);
#4865=VERTEX_POINT('',#17143);
#4866=VERTEX_POINT('',#17146);
#4867=VERTEX_POINT('',#17150);
#4868=VERTEX_POINT('',#17154);
#4869=VERTEX_POINT('',#17158);
#4870=VERTEX_POINT('',#17162);
#4871=VERTEX_POINT('',#17165);
#4872=VERTEX_POINT('',#17169);
#4873=VERTEX_POINT('',#17172);
#4874=VERTEX_POINT('',#17178);
#4875=VERTEX_POINT('',#17182);
#4876=VERTEX_POINT('',#17186);
#4877=VERTEX_POINT('',#17189);
#4878=VERTEX_POINT('',#17193);
#4879=VERTEX_POINT('',#17196);
#4880=VERTEX_POINT('',#17237);
#4881=VERTEX_POINT('',#17283);
#4882=VERTEX_POINT('',#17339);
#4883=VERTEX_POINT('',#17344);
#4884=VERTEX_POINT('',#17411);
#4885=VERTEX_POINT('',#17416);
#4886=VERTEX_POINT('',#17528);
#4887=VERTEX_POINT('',#17532);
#4888=VERTEX_POINT('',#17537);
#4889=VERTEX_POINT('',#17541);
#4890=VERTEX_POINT('',#17555);
#4891=VERTEX_POINT('',#17557);
#4892=VERTEX_POINT('',#17559);
#4893=VERTEX_POINT('',#17563);
#4894=VERTEX_POINT('',#17565);
#4895=VERTEX_POINT('',#17574);
#4896=VERTEX_POINT('',#17582);
#4897=VERTEX_POINT('',#17589);
#4898=VERTEX_POINT('',#17591);
#4899=VERTEX_POINT('',#17600);
#4900=VERTEX_POINT('',#17608);
#4901=VERTEX_POINT('',#17615);
#4902=VERTEX_POINT('',#17617);
#4903=VERTEX_POINT('',#17626);
#4904=VERTEX_POINT('',#17634);
#4905=VERTEX_POINT('',#17641);
#4906=VERTEX_POINT('',#17643);
#4907=VERTEX_POINT('',#17652);
#4908=VERTEX_POINT('',#17660);
#4909=VERTEX_POINT('',#17667);
#4910=VERTEX_POINT('',#17669);
#4911=VERTEX_POINT('',#17678);
#4912=VERTEX_POINT('',#17686);
#4913=VERTEX_POINT('',#17693);
#4914=VERTEX_POINT('',#17695);
#4915=VERTEX_POINT('',#17704);
#4916=VERTEX_POINT('',#17712);
#4917=VERTEX_POINT('',#17719);
#4918=VERTEX_POINT('',#17721);
#4919=VERTEX_POINT('',#17730);
#4920=VERTEX_POINT('',#17738);
#4921=VERTEX_POINT('',#17745);
#4922=VERTEX_POINT('',#17747);
#4923=VERTEX_POINT('',#17756);
#4924=VERTEX_POINT('',#17764);
#4925=VERTEX_POINT('',#17771);
#4926=VERTEX_POINT('',#17773);
#4927=VERTEX_POINT('',#17782);
#4928=VERTEX_POINT('',#17790);
#4929=VERTEX_POINT('',#17797);
#4930=VERTEX_POINT('',#17799);
#4931=VERTEX_POINT('',#17808);
#4932=VERTEX_POINT('',#17816);
#4933=VERTEX_POINT('',#17823);
#4934=VERTEX_POINT('',#17825);
#4935=VERTEX_POINT('',#17834);
#4936=VERTEX_POINT('',#17842);
#4937=VERTEX_POINT('',#17849);
#4938=VERTEX_POINT('',#17851);
#4939=VERTEX_POINT('',#17860);
#4940=VERTEX_POINT('',#17868);
#4941=VERTEX_POINT('',#17875);
#4942=VERTEX_POINT('',#17877);
#4943=VERTEX_POINT('',#17886);
#4944=VERTEX_POINT('',#17894);
#4945=VERTEX_POINT('',#17901);
#4946=VERTEX_POINT('',#17903);
#4947=VERTEX_POINT('',#17912);
#4948=VERTEX_POINT('',#17920);
#4949=VERTEX_POINT('',#17927);
#4950=VERTEX_POINT('',#17929);
#4951=VERTEX_POINT('',#17938);
#4952=VERTEX_POINT('',#17946);
#4953=VERTEX_POINT('',#17953);
#4954=VERTEX_POINT('',#17955);
#4955=VERTEX_POINT('',#17964);
#4956=VERTEX_POINT('',#17972);
#4957=VERTEX_POINT('',#17979);
#4958=VERTEX_POINT('',#17981);
#4959=VERTEX_POINT('',#17990);
#4960=VERTEX_POINT('',#17998);
#4961=VERTEX_POINT('',#18005);
#4962=VERTEX_POINT('',#18007);
#4963=VERTEX_POINT('',#18016);
#4964=VERTEX_POINT('',#18024);
#4965=VERTEX_POINT('',#18031);
#4966=VERTEX_POINT('',#18033);
#4967=VERTEX_POINT('',#18042);
#4968=VERTEX_POINT('',#18050);
#4969=VERTEX_POINT('',#18057);
#4970=VERTEX_POINT('',#18059);
#4971=VERTEX_POINT('',#18068);
#4972=VERTEX_POINT('',#18076);
#4973=VERTEX_POINT('',#18083);
#4974=VERTEX_POINT('',#18090);
#4975=VERTEX_POINT('',#18091);
#4976=VERTEX_POINT('',#18093);
#4977=VERTEX_POINT('',#18131);
#4978=VERTEX_POINT('',#18283);
#4979=VERTEX_POINT('',#18298);
#4980=VERTEX_POINT('',#18311);
#4981=VERTEX_POINT('',#18316);
#4982=VERTEX_POINT('',#18350);
#4983=VERTEX_POINT('',#18380);
#4984=VERTEX_POINT('',#18382);
#4985=VERTEX_POINT('',#18397);
#4986=VERTEX_POINT('',#18414);
#4987=VERTEX_POINT('',#18416);
#4988=VERTEX_POINT('',#18565);
#4989=VERTEX_POINT('',#18578);
#4990=VERTEX_POINT('',#18583);
#4991=VERTEX_POINT('',#18631);
#4992=VERTEX_POINT('',#18632);
#4993=VERTEX_POINT('',#18671);
#4994=VERTEX_POINT('',#18698);
#4995=VERTEX_POINT('',#18699);
#4996=VERTEX_POINT('',#18744);
#4997=VERTEX_POINT('',#18745);
#4998=VERTEX_POINT('',#18792);
#4999=VERTEX_POINT('',#18803);
#5000=VERTEX_POINT('',#18837);
#5001=VERTEX_POINT('',#18838);
#5002=VERTEX_POINT('',#18883);
#5003=VERTEX_POINT('',#18922);
#5004=VERTEX_POINT('',#18956);
#5005=VERTEX_POINT('',#18957);
#5006=VERTEX_POINT('',#19002);
#5007=VERTEX_POINT('',#19041);
#5008=VERTEX_POINT('',#19075);
#5009=VERTEX_POINT('',#19076);
#5010=VERTEX_POINT('',#19121);
#5011=VERTEX_POINT('',#19160);
#5012=VERTEX_POINT('',#19194);
#5013=VERTEX_POINT('',#19195);
#5014=VERTEX_POINT('',#19240);
#5015=VERTEX_POINT('',#19279);
#5016=VERTEX_POINT('',#19313);
#5017=VERTEX_POINT('',#19314);
#5018=VERTEX_POINT('',#19359);
#5019=VERTEX_POINT('',#19398);
#5020=VERTEX_POINT('',#19432);
#5021=VERTEX_POINT('',#19433);
#5022=VERTEX_POINT('',#19478);
#5023=VERTEX_POINT('',#19517);
#5024=VERTEX_POINT('',#19551);
#5025=VERTEX_POINT('',#19552);
#5026=VERTEX_POINT('',#19597);
#5027=VERTEX_POINT('',#19636);
#5028=VERTEX_POINT('',#19670);
#5029=VERTEX_POINT('',#19671);
#5030=VERTEX_POINT('',#19716);
#5031=VERTEX_POINT('',#19755);
#5032=VERTEX_POINT('',#19789);
#5033=VERTEX_POINT('',#19790);
#5034=VERTEX_POINT('',#19803);
#5035=VERTEX_POINT('',#19840);
#5036=VERTEX_POINT('',#19879);
#5037=VERTEX_POINT('',#19913);
#5038=VERTEX_POINT('',#19914);
#5039=VERTEX_POINT('',#19959);
#5040=VERTEX_POINT('',#19998);
#5041=VERTEX_POINT('',#20032);
#5042=VERTEX_POINT('',#20033);
#5043=VERTEX_POINT('',#20078);
#5044=VERTEX_POINT('',#20117);
#5045=VERTEX_POINT('',#20151);
#5046=VERTEX_POINT('',#20152);
#5047=VERTEX_POINT('',#20197);
#5048=VERTEX_POINT('',#20236);
#5049=VERTEX_POINT('',#20270);
#5050=VERTEX_POINT('',#20271);
#5051=VERTEX_POINT('',#20316);
#5052=VERTEX_POINT('',#20355);
#5053=VERTEX_POINT('',#20389);
#5054=VERTEX_POINT('',#20390);
#5055=VERTEX_POINT('',#20435);
#5056=VERTEX_POINT('',#20474);
#5057=VERTEX_POINT('',#20508);
#5058=VERTEX_POINT('',#20509);
#5059=VERTEX_POINT('',#20554);
#5060=VERTEX_POINT('',#20593);
#5061=VERTEX_POINT('',#20627);
#5062=VERTEX_POINT('',#20628);
#5063=VERTEX_POINT('',#20673);
#5064=VERTEX_POINT('',#20712);
#5065=VERTEX_POINT('',#20746);
#5066=VERTEX_POINT('',#20747);
#5067=VERTEX_POINT('',#20792);
#5068=VERTEX_POINT('',#20831);
#5069=VERTEX_POINT('',#20865);
#5070=VERTEX_POINT('',#20896);
#5071=VERTEX_POINT('',#20934);
#5072=VERTEX_POINT('',#20973);
#5073=VERTEX_POINT('',#20980);
#5074=VERTEX_POINT('',#21013);
#5075=VERTEX_POINT('',#21058);
#5076=VERTEX_POINT('',#21064);
#5077=VERTEX_POINT('',#21067);
#5078=VERTEX_POINT('',#21071);
#5079=VERTEX_POINT('',#21075);
#5080=VERTEX_POINT('',#21081);
#5081=VERTEX_POINT('',#21083);
#5082=VERTEX_POINT('',#21085);
#5083=VERTEX_POINT('',#21089);
#5084=VERTEX_POINT('',#21093);
#5085=VERTEX_POINT('',#21096);
#5086=VERTEX_POINT('',#21099);
#5087=VERTEX_POINT('',#21100);
#5088=VERTEX_POINT('',#21104);
#5089=VERTEX_POINT('',#21105);
#5090=VERTEX_POINT('',#21112);
#5091=VERTEX_POINT('',#21113);
#5092=VERTEX_POINT('',#21117);
#5093=VERTEX_POINT('',#21119);
#5094=VERTEX_POINT('',#21125);
#5095=VERTEX_POINT('',#21128);
#5096=VERTEX_POINT('',#21132);
#5097=VERTEX_POINT('',#21136);
#5098=VERTEX_POINT('',#21139);
#5099=VERTEX_POINT('',#21143);
#5100=VERTEX_POINT('',#21146);
#5101=VERTEX_POINT('',#21268);
#5102=VERTEX_POINT('',#21269);
#5103=VERTEX_POINT('',#21304);
#5104=VERTEX_POINT('',#21319);
#5105=VERTEX_POINT('',#21332);
#5106=VERTEX_POINT('',#21337);
#5107=VERTEX_POINT('',#21371);
#5108=VERTEX_POINT('',#21401);
#5109=VERTEX_POINT('',#21403);
#5110=VERTEX_POINT('',#21405);
#5111=VERTEX_POINT('',#21420);
#5112=VERTEX_POINT('',#21422);
#5113=VERTEX_POINT('',#21439);
#5114=VERTEX_POINT('',#21441);
#5115=VERTEX_POINT('',#21627);
#5116=VERTEX_POINT('',#21640);
#5117=VERTEX_POINT('',#21645);
#5118=VERTEX_POINT('',#21693);
#5119=VERTEX_POINT('',#21694);
#5120=VERTEX_POINT('',#21733);
#5121=VERTEX_POINT('',#21760);
#5122=VERTEX_POINT('',#21761);
#5123=VERTEX_POINT('',#21768);
#5124=VERTEX_POINT('',#21775);
#5125=VERTEX_POINT('',#21816);
#5126=VERTEX_POINT('',#21817);
#5127=VERTEX_POINT('',#21826);
#5128=VERTEX_POINT('',#21835);
#5129=VERTEX_POINT('',#21879);
#5130=VERTEX_POINT('',#21881);
#5131=VERTEX_POINT('',#21883);
#5132=VERTEX_POINT('',#21888);
#5133=VERTEX_POINT('',#21890);
#5134=VERTEX_POINT('',#21899);
#5135=VERTEX_POINT('',#21907);
#5136=VERTEX_POINT('',#21914);
#5137=VERTEX_POINT('',#21916);
#5138=VERTEX_POINT('',#21925);
#5139=VERTEX_POINT('',#21933);
#5140=VERTEX_POINT('',#21940);
#5141=VERTEX_POINT('',#21942);
#5142=VERTEX_POINT('',#21951);
#5143=VERTEX_POINT('',#21959);
#5144=VERTEX_POINT('',#21966);
#5145=VERTEX_POINT('',#21968);
#5146=VERTEX_POINT('',#21977);
#5147=VERTEX_POINT('',#21985);
#5148=VERTEX_POINT('',#21992);
#5149=VERTEX_POINT('',#21994);
#5150=VERTEX_POINT('',#22003);
#5151=VERTEX_POINT('',#22011);
#5152=VERTEX_POINT('',#22018);
#5153=VERTEX_POINT('',#22020);
#5154=VERTEX_POINT('',#22029);
#5155=VERTEX_POINT('',#22037);
#5156=VERTEX_POINT('',#22044);
#5157=VERTEX_POINT('',#22046);
#5158=VERTEX_POINT('',#22055);
#5159=VERTEX_POINT('',#22063);
#5160=VERTEX_POINT('',#22070);
#5161=VERTEX_POINT('',#22072);
#5162=VERTEX_POINT('',#22081);
#5163=VERTEX_POINT('',#22089);
#5164=VERTEX_POINT('',#22096);
#5165=VERTEX_POINT('',#22098);
#5166=VERTEX_POINT('',#22107);
#5167=VERTEX_POINT('',#22115);
#5168=VERTEX_POINT('',#22123);
#5169=VERTEX_POINT('',#22125);
#5170=VERTEX_POINT('',#22134);
#5171=VERTEX_POINT('',#22142);
#5172=VERTEX_POINT('',#22149);
#5173=VERTEX_POINT('',#22151);
#5174=VERTEX_POINT('',#22160);
#5175=VERTEX_POINT('',#22168);
#5176=VERTEX_POINT('',#22175);
#5177=VERTEX_POINT('',#22177);
#5178=VERTEX_POINT('',#22186);
#5179=VERTEX_POINT('',#22194);
#5180=VERTEX_POINT('',#22201);
#5181=VERTEX_POINT('',#22203);
#5182=VERTEX_POINT('',#22212);
#5183=VERTEX_POINT('',#22220);
#5184=VERTEX_POINT('',#22227);
#5185=VERTEX_POINT('',#22229);
#5186=VERTEX_POINT('',#22238);
#5187=VERTEX_POINT('',#22246);
#5188=VERTEX_POINT('',#22253);
#5189=VERTEX_POINT('',#22255);
#5190=VERTEX_POINT('',#22264);
#5191=VERTEX_POINT('',#22272);
#5192=VERTEX_POINT('',#22279);
#5193=VERTEX_POINT('',#22281);
#5194=VERTEX_POINT('',#22290);
#5195=VERTEX_POINT('',#22298);
#5196=VERTEX_POINT('',#22305);
#5197=VERTEX_POINT('',#22307);
#5198=VERTEX_POINT('',#22316);
#5199=VERTEX_POINT('',#22324);
#5200=VERTEX_POINT('',#22331);
#5201=VERTEX_POINT('',#22333);
#5202=VERTEX_POINT('',#22342);
#5203=VERTEX_POINT('',#22350);
#5204=VERTEX_POINT('',#22357);
#5205=VERTEX_POINT('',#22359);
#5206=VERTEX_POINT('',#22368);
#5207=VERTEX_POINT('',#22383);
#5208=VERTEX_POINT('',#22394);
#5209=VERTEX_POINT('',#22428);
#5210=VERTEX_POINT('',#22429);
#5211=VERTEX_POINT('',#22474);
#5212=VERTEX_POINT('',#22513);
#5213=VERTEX_POINT('',#22547);
#5214=VERTEX_POINT('',#22548);
#5215=VERTEX_POINT('',#22593);
#5216=VERTEX_POINT('',#22632);
#5217=VERTEX_POINT('',#22666);
#5218=VERTEX_POINT('',#22667);
#5219=VERTEX_POINT('',#22712);
#5220=VERTEX_POINT('',#22751);
#5221=VERTEX_POINT('',#22785);
#5222=VERTEX_POINT('',#22786);
#5223=VERTEX_POINT('',#22831);
#5224=VERTEX_POINT('',#22870);
#5225=VERTEX_POINT('',#22904);
#5226=VERTEX_POINT('',#22905);
#5227=VERTEX_POINT('',#22950);
#5228=VERTEX_POINT('',#22989);
#5229=VERTEX_POINT('',#23023);
#5230=VERTEX_POINT('',#23024);
#5231=VERTEX_POINT('',#23069);
#5232=VERTEX_POINT('',#23108);
#5233=VERTEX_POINT('',#23142);
#5234=VERTEX_POINT('',#23143);
#5235=VERTEX_POINT('',#23188);
#5236=VERTEX_POINT('',#23227);
#5237=VERTEX_POINT('',#23261);
#5238=VERTEX_POINT('',#23262);
#5239=VERTEX_POINT('',#23307);
#5240=VERTEX_POINT('',#23346);
#5241=VERTEX_POINT('',#23380);
#5242=VERTEX_POINT('',#23381);
#5243=VERTEX_POINT('',#23426);
#5244=VERTEX_POINT('',#23431);
#5245=VERTEX_POINT('',#23470);
#5246=VERTEX_POINT('',#23504);
#5247=VERTEX_POINT('',#23505);
#5248=VERTEX_POINT('',#23550);
#5249=VERTEX_POINT('',#23589);
#5250=VERTEX_POINT('',#23623);
#5251=VERTEX_POINT('',#23624);
#5252=VERTEX_POINT('',#23669);
#5253=VERTEX_POINT('',#23708);
#5254=VERTEX_POINT('',#23742);
#5255=VERTEX_POINT('',#23743);
#5256=VERTEX_POINT('',#23788);
#5257=VERTEX_POINT('',#23827);
#5258=VERTEX_POINT('',#23861);
#5259=VERTEX_POINT('',#23862);
#5260=VERTEX_POINT('',#23907);
#5261=VERTEX_POINT('',#23946);
#5262=VERTEX_POINT('',#23980);
#5263=VERTEX_POINT('',#23981);
#5264=VERTEX_POINT('',#24026);
#5265=VERTEX_POINT('',#24065);
#5266=VERTEX_POINT('',#24099);
#5267=VERTEX_POINT('',#24100);
#5268=VERTEX_POINT('',#24145);
#5269=VERTEX_POINT('',#24184);
#5270=VERTEX_POINT('',#24218);
#5271=VERTEX_POINT('',#24219);
#5272=VERTEX_POINT('',#24264);
#5273=VERTEX_POINT('',#24303);
#5274=VERTEX_POINT('',#24337);
#5275=VERTEX_POINT('',#24338);
#5276=VERTEX_POINT('',#24383);
#5277=VERTEX_POINT('',#24422);
#5278=VERTEX_POINT('',#24456);
#5279=VERTEX_POINT('',#24487);
#5280=VERTEX_POINT('',#24525);
#5281=VERTEX_POINT('',#24564);
#5282=VERTEX_POINT('',#24571);
#5283=VERTEX_POINT('',#24604);
#5284=VERTEX_POINT('',#24649);
#5285=VERTEX_POINT('',#24656);
#5286=VERTEX_POINT('',#24659);
#5287=VERTEX_POINT('',#24663);
#5288=VERTEX_POINT('',#24667);
#5289=VERTEX_POINT('',#24673);
#5290=VERTEX_POINT('',#24675);
#5291=VERTEX_POINT('',#24678);
#5292=VERTEX_POINT('',#24680);
#5293=VERTEX_POINT('',#24685);
#5294=VERTEX_POINT('',#24689);
#5295=VERTEX_POINT('',#24691);
#5296=VERTEX_POINT('',#24694);
#5297=VERTEX_POINT('',#24696);
#5298=VERTEX_POINT('',#24701);
#5299=VERTEX_POINT('',#24702);
#5300=VERTEX_POINT('',#24709);
#5301=VERTEX_POINT('',#24711);
#5302=VERTEX_POINT('',#24718);
#5303=VERTEX_POINT('',#24720);
#5304=VERTEX_POINT('',#24727);
#5305=VERTEX_POINT('',#24729);
#5306=VERTEX_POINT('',#24736);
#5307=VERTEX_POINT('',#24738);
#5308=VERTEX_POINT('',#24745);
#5309=VERTEX_POINT('',#24748);
#5310=VERTEX_POINT('',#24750);
#5311=VERTEX_POINT('',#24757);
#5312=VERTEX_POINT('',#24759);
#5313=VERTEX_POINT('',#24768);
#5314=VERTEX_POINT('',#24769);
#5315=VERTEX_POINT('',#24774);
#5316=VERTEX_POINT('',#24797);
#5317=VERTEX_POINT('',#24802);
#5318=VERTEX_POINT('',#24804);
#5319=VERTEX_POINT('',#24809);
#5320=VERTEX_POINT('',#24836);
#5321=VERTEX_POINT('',#24838);
#5322=VERTEX_POINT('',#24862);
#5323=VERTEX_POINT('',#24893);
#5324=VERTEX_POINT('',#24895);
#5325=VERTEX_POINT('',#24897);
#5326=VERTEX_POINT('',#24904);
#5327=VERTEX_POINT('',#24906);
#5328=VERTEX_POINT('',#24913);
#5329=VERTEX_POINT('',#24915);
#5330=VERTEX_POINT('',#24922);
#5331=VERTEX_POINT('',#24924);
#5332=VERTEX_POINT('',#24932);
#5333=VERTEX_POINT('',#24934);
#5334=VERTEX_POINT('',#24941);
#5335=VERTEX_POINT('',#24943);
#5336=VERTEX_POINT('',#24976);
#5337=VERTEX_POINT('',#24978);
#5338=VERTEX_POINT('',#24983);
#5339=VERTEX_POINT('',#24988);
#5340=VERTEX_POINT('',#24990);
#5341=VERTEX_POINT('',#24995);
#5342=VERTEX_POINT('',#25000);
#5343=VERTEX_POINT('',#25002);
#5344=VERTEX_POINT('',#25005);
#5345=VERTEX_POINT('',#25007);
#5346=VERTEX_POINT('',#25012);
#5347=VERTEX_POINT('',#25017);
#5348=VERTEX_POINT('',#25019);
#5349=VERTEX_POINT('',#25024);
#5350=VERTEX_POINT('',#25029);
#5351=VERTEX_POINT('',#25031);
#5352=VERTEX_POINT('',#25036);
#5353=VERTEX_POINT('',#25041);
#5354=VERTEX_POINT('',#25043);
#5355=VERTEX_POINT('',#25048);
#5356=VERTEX_POINT('',#25055);
#5357=VERTEX_POINT('',#25080);
#5358=VERTEX_POINT('',#25081);
#5359=VERTEX_POINT('',#25108);
#5360=VERTEX_POINT('',#25114);
#5361=VERTEX_POINT('',#25164);
#5362=VERTEX_POINT('',#25189);
#5363=VERTEX_POINT('',#25190);
#5364=VERTEX_POINT('',#25217);
#5365=VERTEX_POINT('',#25223);
#5366=VERTEX_POINT('',#25273);
#5367=VERTEX_POINT('',#25275);
#5368=VERTEX_POINT('',#25300);
#5369=VERTEX_POINT('',#25301);
#5370=VERTEX_POINT('',#25328);
#5371=VERTEX_POINT('',#25334);
#5372=VERTEX_POINT('',#25384);
#5373=VERTEX_POINT('',#25409);
#5374=VERTEX_POINT('',#25410);
#5375=VERTEX_POINT('',#25437);
#5376=VERTEX_POINT('',#25443);
#5377=VERTEX_POINT('',#25493);
#5378=VERTEX_POINT('',#25518);
#5379=VERTEX_POINT('',#25523);
#5380=VERTEX_POINT('',#25525);
#5381=VERTEX_POINT('',#25552);
#5382=VERTEX_POINT('',#25578);
#5383=VERTEX_POINT('',#25606);
#5384=VERTEX_POINT('',#25609);
#5385=VERTEX_POINT('',#25611);
#5386=VERTEX_POINT('',#25616);
#5387=VERTEX_POINT('',#25646);
#5388=VERTEX_POINT('',#25670);
#5389=VERTEX_POINT('',#25697);
#5390=VERTEX_POINT('',#25700);
#5391=VERTEX_POINT('',#25704);
#5392=VERTEX_POINT('',#25708);
#5393=VERTEX_POINT('',#25714);
#5394=VERTEX_POINT('',#25716);
#5395=VERTEX_POINT('',#25720);
#5396=VERTEX_POINT('',#25725);
#5397=VERTEX_POINT('',#25731);
#5398=VERTEX_POINT('',#25733);
#5399=VERTEX_POINT('',#25737);
#5400=VERTEX_POINT('',#25740);
#5401=VERTEX_POINT('',#25746);
#5402=VERTEX_POINT('',#25747);
#5403=VERTEX_POINT('',#25749);
#5404=VERTEX_POINT('',#25751);
#5405=VERTEX_POINT('',#25755);
#5406=VERTEX_POINT('',#25757);
#5407=VERTEX_POINT('',#25761);
#5408=VERTEX_POINT('',#25763);
#5409=VERTEX_POINT('',#25765);
#5410=VERTEX_POINT('',#25769);
#5411=VERTEX_POINT('',#25770);
#5412=VERTEX_POINT('',#25772);
#5413=VERTEX_POINT('',#25774);
#5414=VERTEX_POINT('',#25778);
#5415=VERTEX_POINT('',#25780);
#5416=VERTEX_POINT('',#25784);
#5417=VERTEX_POINT('',#25786);
#5418=VERTEX_POINT('',#25793);
#5419=VERTEX_POINT('',#25795);
#5420=VERTEX_POINT('',#25797);
#5421=VERTEX_POINT('',#25799);
#5422=VERTEX_POINT('',#25801);
#5423=VERTEX_POINT('',#25803);
#5424=VERTEX_POINT('',#25806);
#5425=VERTEX_POINT('',#25808);
#5426=VERTEX_POINT('',#25813);
#5427=VERTEX_POINT('',#25817);
#5428=VERTEX_POINT('',#25821);
#5429=VERTEX_POINT('',#25825);
#5430=VERTEX_POINT('',#25827);
#5431=VERTEX_POINT('',#25833);
#5432=VERTEX_POINT('',#25835);
#5433=VERTEX_POINT('',#25845);
#5434=VERTEX_POINT('',#25846);
#5435=VERTEX_POINT('',#25848);
#5436=VERTEX_POINT('',#25859);
#5437=VERTEX_POINT('',#25869);
#5438=VERTEX_POINT('',#25870);
#5439=VERTEX_POINT('',#25917);
#5440=VERTEX_POINT('',#25918);
#5441=VERTEX_POINT('',#25965);
#5442=VERTEX_POINT('',#25966);
#5443=VERTEX_POINT('',#26019);
#5444=VERTEX_POINT('',#26020);
#5445=VERTEX_POINT('',#26067);
#5446=VERTEX_POINT('',#26068);
#5447=VERTEX_POINT('',#26121);
#5448=VERTEX_POINT('',#26122);
#5449=VERTEX_POINT('',#26124);
#5450=VERTEX_POINT('',#26131);
#5451=VERTEX_POINT('',#26132);
#5452=VERTEX_POINT('',#26145);
#5453=VERTEX_POINT('',#26157);
#5454=VERTEX_POINT('',#26158);
#5455=VERTEX_POINT('',#26182);
#5456=VERTEX_POINT('',#26183);
#5457=VERTEX_POINT('',#26207);
#5458=VERTEX_POINT('',#26208);
#5459=VERTEX_POINT('',#26232);
#5460=VERTEX_POINT('',#26233);
#5461=VERTEX_POINT('',#26256);
#5462=VERTEX_POINT('',#26309);
#5463=VERTEX_POINT('',#26311);
#5464=VERTEX_POINT('',#26549);
#5465=VERTEX_POINT('',#26612);
#5466=VERTEX_POINT('',#26615);
#5467=VERTEX_POINT('',#26860);
#5468=VERTEX_POINT('',#26861);
#5469=VERTEX_POINT('',#26863);
#5470=VERTEX_POINT('',#26865);
#5471=VERTEX_POINT('',#26869);
#5472=VERTEX_POINT('',#26871);
#5473=VERTEX_POINT('',#26875);
#5474=VERTEX_POINT('',#26877);
#5475=VERTEX_POINT('',#26881);
#5476=VERTEX_POINT('',#26883);
#5477=VERTEX_POINT('',#26887);
#5478=VERTEX_POINT('',#26889);
#5479=VERTEX_POINT('',#26897);
#5480=VERTEX_POINT('',#26904);
#5481=VERTEX_POINT('',#26910);
#5482=VERTEX_POINT('',#26911);
#5483=VERTEX_POINT('',#26913);
#5484=VERTEX_POINT('',#26924);
#5485=VERTEX_POINT('',#26934);
#5486=VERTEX_POINT('',#26935);
#5487=VERTEX_POINT('',#26982);
#5488=VERTEX_POINT('',#26983);
#5489=VERTEX_POINT('',#27030);
#5490=VERTEX_POINT('',#27031);
#5491=VERTEX_POINT('',#27081);
#5492=VERTEX_POINT('',#27082);
#5493=VERTEX_POINT('',#27132);
#5494=VERTEX_POINT('',#27133);
#5495=VERTEX_POINT('',#27180);
#5496=VERTEX_POINT('',#27181);
#5497=VERTEX_POINT('',#27228);
#5498=VERTEX_POINT('',#27229);
#5499=VERTEX_POINT('',#27282);
#5500=VERTEX_POINT('',#27283);
#5501=VERTEX_POINT('',#27330);
#5502=VERTEX_POINT('',#27331);
#5503=VERTEX_POINT('',#27378);
#5504=VERTEX_POINT('',#27379);
#5505=VERTEX_POINT('',#27432);
#5506=VERTEX_POINT('',#27433);
#5507=VERTEX_POINT('',#27480);
#5508=VERTEX_POINT('',#27481);
#5509=VERTEX_POINT('',#27528);
#5510=VERTEX_POINT('',#27529);
#5511=VERTEX_POINT('',#27576);
#5512=VERTEX_POINT('',#27577);
#5513=VERTEX_POINT('',#27630);
#5514=VERTEX_POINT('',#27631);
#5515=VERTEX_POINT('',#27678);
#5516=VERTEX_POINT('',#27679);
#5517=VERTEX_POINT('',#27726);
#5518=VERTEX_POINT('',#27727);
#5519=VERTEX_POINT('',#27780);
#5520=VERTEX_POINT('',#27781);
#5521=VERTEX_POINT('',#27828);
#5522=VERTEX_POINT('',#27829);
#5523=VERTEX_POINT('',#27876);
#5524=VERTEX_POINT('',#27877);
#5525=VERTEX_POINT('',#27927);
#5526=VERTEX_POINT('',#27928);
#5527=VERTEX_POINT('',#27975);
#5528=VERTEX_POINT('',#27976);
#5529=VERTEX_POINT('',#28023);
#5530=VERTEX_POINT('',#28024);
#5531=VERTEX_POINT('',#28071);
#5532=VERTEX_POINT('',#28072);
#5533=VERTEX_POINT('',#28074);
#5534=VERTEX_POINT('',#28081);
#5535=VERTEX_POINT('',#28082);
#5536=VERTEX_POINT('',#28094);
#5537=VERTEX_POINT('',#28106);
#5538=VERTEX_POINT('',#28107);
#5539=VERTEX_POINT('',#28130);
#5540=VERTEX_POINT('',#28131);
#5541=VERTEX_POINT('',#28154);
#5542=VERTEX_POINT('',#28155);
#5543=VERTEX_POINT('',#28179);
#5544=VERTEX_POINT('',#28180);
#5545=VERTEX_POINT('',#28204);
#5546=VERTEX_POINT('',#28205);
#5547=VERTEX_POINT('',#28228);
#5548=VERTEX_POINT('',#28229);
#5549=VERTEX_POINT('',#28253);
#5550=VERTEX_POINT('',#28254);
#5551=VERTEX_POINT('',#28278);
#5552=VERTEX_POINT('',#28279);
#5553=VERTEX_POINT('',#28302);
#5554=VERTEX_POINT('',#28303);
#5555=VERTEX_POINT('',#28327);
#5556=VERTEX_POINT('',#28328);
#5557=VERTEX_POINT('',#28352);
#5558=VERTEX_POINT('',#28353);
#5559=VERTEX_POINT('',#28376);
#5560=VERTEX_POINT('',#28377);
#5561=VERTEX_POINT('',#28400);
#5562=VERTEX_POINT('',#28401);
#5563=VERTEX_POINT('',#28425);
#5564=VERTEX_POINT('',#28426);
#5565=VERTEX_POINT('',#28450);
#5566=VERTEX_POINT('',#28451);
#5567=VERTEX_POINT('',#28474);
#5568=VERTEX_POINT('',#28475);
#5569=VERTEX_POINT('',#28499);
#5570=VERTEX_POINT('',#28500);
#5571=VERTEX_POINT('',#28524);
#5572=VERTEX_POINT('',#28525);
#5573=VERTEX_POINT('',#28548);
#5574=VERTEX_POINT('',#28549);
#5575=VERTEX_POINT('',#28573);
#5576=VERTEX_POINT('',#28574);
#5577=VERTEX_POINT('',#28597);
#5578=VERTEX_POINT('',#28598);
#5579=VERTEX_POINT('',#28622);
#5580=VERTEX_POINT('',#28623);
#5581=VERTEX_POINT('',#29261);
#5582=VERTEX_POINT('',#29333);
#5583=VERTEX_POINT('',#29399);
#5584=VERTEX_POINT('',#29402);
#5585=VERTEX_POINT('',#30087);
#5586=VERTEX_POINT('',#30154);
#5587=VERTEX_POINT('',#30155);
#5588=VERTEX_POINT('',#30159);
#5589=VERTEX_POINT('',#30160);
#5590=VERTEX_POINT('',#30162);
#5591=VERTEX_POINT('',#30164);
#5592=VERTEX_POINT('',#30168);
#5593=VERTEX_POINT('',#30170);
#5594=VERTEX_POINT('',#30174);
#5595=VERTEX_POINT('',#30176);
#5596=VERTEX_POINT('',#30180);
#5597=VERTEX_POINT('',#30182);
#5598=VERTEX_POINT('',#30186);
#5599=VERTEX_POINT('',#30188);
#5600=VERTEX_POINT('',#30196);
#5601=VERTEX_POINT('',#30197);
#5602=VERTEX_POINT('',#30199);
#5603=VERTEX_POINT('',#30201);
#5604=VERTEX_POINT('',#30205);
#5605=VERTEX_POINT('',#30209);
#5606=VERTEX_POINT('',#30215);
#5607=VERTEX_POINT('',#30216);
#5608=VERTEX_POINT('',#30218);
#5609=VERTEX_POINT('',#30220);
#5610=VERTEX_POINT('',#30224);
#5611=VERTEX_POINT('',#30228);
#5612=VERTEX_POINT('',#30234);
#5613=VERTEX_POINT('',#30235);
#5614=VERTEX_POINT('',#30237);
#5615=VERTEX_POINT('',#30239);
#5616=VERTEX_POINT('',#30243);
#5617=VERTEX_POINT('',#30247);
#5618=VERTEX_POINT('',#30253);
#5619=VERTEX_POINT('',#30254);
#5620=VERTEX_POINT('',#30256);
#5621=VERTEX_POINT('',#30258);
#5622=VERTEX_POINT('',#30262);
#5623=VERTEX_POINT('',#30266);
#5624=VERTEX_POINT('',#30272);
#5625=VERTEX_POINT('',#30273);
#5626=VERTEX_POINT('',#30275);
#5627=VERTEX_POINT('',#30277);
#5628=VERTEX_POINT('',#30281);
#5629=VERTEX_POINT('',#30285);
#5630=VERTEX_POINT('',#30291);
#5631=VERTEX_POINT('',#30292);
#5632=VERTEX_POINT('',#30294);
#5633=VERTEX_POINT('',#30296);
#5634=VERTEX_POINT('',#30300);
#5635=VERTEX_POINT('',#30304);
#5636=VERTEX_POINT('',#30310);
#5637=VERTEX_POINT('',#30311);
#5638=VERTEX_POINT('',#30313);
#5639=VERTEX_POINT('',#30315);
#5640=VERTEX_POINT('',#30319);
#5641=VERTEX_POINT('',#30323);
#5642=VERTEX_POINT('',#30329);
#5643=VERTEX_POINT('',#30330);
#5644=VERTEX_POINT('',#30332);
#5645=VERTEX_POINT('',#30334);
#5646=VERTEX_POINT('',#30338);
#5647=VERTEX_POINT('',#30342);
#5648=VERTEX_POINT('',#30348);
#5649=VERTEX_POINT('',#30349);
#5650=VERTEX_POINT('',#30351);
#5651=VERTEX_POINT('',#30353);
#5652=VERTEX_POINT('',#30357);
#5653=VERTEX_POINT('',#30359);
#5654=VERTEX_POINT('',#30363);
#5655=VERTEX_POINT('',#30367);
#5656=VERTEX_POINT('',#30371);
#5657=VERTEX_POINT('',#30372);
#5658=VERTEX_POINT('',#30374);
#5659=VERTEX_POINT('',#30376);
#5660=VERTEX_POINT('',#30380);
#5661=VERTEX_POINT('',#30384);
#5662=VERTEX_POINT('',#30390);
#5663=VERTEX_POINT('',#30391);
#5664=VERTEX_POINT('',#30393);
#5665=VERTEX_POINT('',#30395);
#5666=VERTEX_POINT('',#30399);
#5667=VERTEX_POINT('',#30403);
#5668=VERTEX_POINT('',#30409);
#5669=VERTEX_POINT('',#30410);
#5670=VERTEX_POINT('',#30412);
#5671=VERTEX_POINT('',#30414);
#5672=VERTEX_POINT('',#30418);
#5673=VERTEX_POINT('',#30422);
#5674=VERTEX_POINT('',#30428);
#5675=VERTEX_POINT('',#30429);
#5676=VERTEX_POINT('',#30431);
#5677=VERTEX_POINT('',#30433);
#5678=VERTEX_POINT('',#30437);
#5679=VERTEX_POINT('',#30441);
#5680=VERTEX_POINT('',#30447);
#5681=VERTEX_POINT('',#30448);
#5682=VERTEX_POINT('',#30450);
#5683=VERTEX_POINT('',#30452);
#5684=VERTEX_POINT('',#30456);
#5685=VERTEX_POINT('',#30460);
#5686=VERTEX_POINT('',#30466);
#5687=VERTEX_POINT('',#30467);
#5688=VERTEX_POINT('',#30469);
#5689=VERTEX_POINT('',#30471);
#5690=VERTEX_POINT('',#30475);
#5691=VERTEX_POINT('',#30479);
#5692=VERTEX_POINT('',#30485);
#5693=VERTEX_POINT('',#30486);
#5694=VERTEX_POINT('',#30488);
#5695=VERTEX_POINT('',#30490);
#5696=VERTEX_POINT('',#30494);
#5697=VERTEX_POINT('',#30498);
#5698=VERTEX_POINT('',#30504);
#5699=VERTEX_POINT('',#30505);
#5700=VERTEX_POINT('',#30507);
#5701=VERTEX_POINT('',#30509);
#5702=VERTEX_POINT('',#30513);
#5703=VERTEX_POINT('',#30517);
#5704=VERTEX_POINT('',#30523);
#5705=VERTEX_POINT('',#30524);
#5706=VERTEX_POINT('',#30526);
#5707=VERTEX_POINT('',#30528);
#5708=VERTEX_POINT('',#30532);
#5709=VERTEX_POINT('',#30536);
#5710=VERTEX_POINT('',#30542);
#5711=VERTEX_POINT('',#30543);
#5712=VERTEX_POINT('',#30545);
#5713=VERTEX_POINT('',#30547);
#5714=VERTEX_POINT('',#30551);
#5715=VERTEX_POINT('',#30555);
#5716=VERTEX_POINT('',#30561);
#5717=VERTEX_POINT('',#30562);
#5718=VERTEX_POINT('',#30564);
#5719=VERTEX_POINT('',#30566);
#5720=VERTEX_POINT('',#30570);
#5721=VERTEX_POINT('',#30574);
#5722=VERTEX_POINT('',#30580);
#5723=VERTEX_POINT('',#30581);
#5724=VERTEX_POINT('',#30583);
#5725=VERTEX_POINT('',#30585);
#5726=VERTEX_POINT('',#30589);
#5727=VERTEX_POINT('',#30593);
#5728=VERTEX_POINT('',#30599);
#5729=VERTEX_POINT('',#30600);
#5730=VERTEX_POINT('',#30602);
#5731=VERTEX_POINT('',#30604);
#5732=VERTEX_POINT('',#30608);
#5733=VERTEX_POINT('',#30612);
#5734=VERTEX_POINT('',#30618);
#5735=VERTEX_POINT('',#30619);
#5736=VERTEX_POINT('',#30621);
#5737=VERTEX_POINT('',#30623);
#5738=VERTEX_POINT('',#30627);
#5739=VERTEX_POINT('',#30631);
#5740=VERTEX_POINT('',#30637);
#5741=VERTEX_POINT('',#30638);
#5742=VERTEX_POINT('',#30640);
#5743=VERTEX_POINT('',#30642);
#5744=VERTEX_POINT('',#30646);
#5745=VERTEX_POINT('',#30650);
#5746=VERTEX_POINT('',#30656);
#5747=VERTEX_POINT('',#30657);
#5748=VERTEX_POINT('',#30659);
#5749=VERTEX_POINT('',#30661);
#5750=VERTEX_POINT('',#30665);
#5751=VERTEX_POINT('',#30669);
#5752=VERTEX_POINT('',#30675);
#5753=VERTEX_POINT('',#30676);
#5754=VERTEX_POINT('',#30678);
#5755=VERTEX_POINT('',#30680);
#5756=VERTEX_POINT('',#30684);
#5757=VERTEX_POINT('',#30688);
#5758=VERTEX_POINT('',#30694);
#5759=VERTEX_POINT('',#30695);
#5760=VERTEX_POINT('',#30697);
#5761=VERTEX_POINT('',#30701);
#5762=VERTEX_POINT('',#30703);
#5763=VERTEX_POINT('',#30707);
#5764=VERTEX_POINT('',#30713);
#5765=VERTEX_POINT('',#30714);
#5766=VERTEX_POINT('',#30716);
#5767=VERTEX_POINT('',#30718);
#5768=VERTEX_POINT('',#30722);
#5769=VERTEX_POINT('',#30726);
#5770=VERTEX_POINT('',#30732);
#5771=VERTEX_POINT('',#30733);
#5772=VERTEX_POINT('',#30735);
#5773=VERTEX_POINT('',#30737);
#5774=VERTEX_POINT('',#30741);
#5775=VERTEX_POINT('',#30745);
#5776=VERTEX_POINT('',#30751);
#5777=VERTEX_POINT('',#30752);
#5778=VERTEX_POINT('',#30754);
#5779=VERTEX_POINT('',#30756);
#5780=VERTEX_POINT('',#30760);
#5781=VERTEX_POINT('',#30764);
#5782=VERTEX_POINT('',#30770);
#5783=VERTEX_POINT('',#30771);
#5784=VERTEX_POINT('',#30773);
#5785=VERTEX_POINT('',#30775);
#5786=VERTEX_POINT('',#30779);
#5787=VERTEX_POINT('',#30783);
#5788=VERTEX_POINT('',#30789);
#5789=VERTEX_POINT('',#30790);
#5790=VERTEX_POINT('',#30792);
#5791=VERTEX_POINT('',#30794);
#5792=VERTEX_POINT('',#30798);
#5793=VERTEX_POINT('',#30802);
#5794=VERTEX_POINT('',#30808);
#5795=VERTEX_POINT('',#30809);
#5796=VERTEX_POINT('',#30811);
#5797=VERTEX_POINT('',#30813);
#5798=VERTEX_POINT('',#30817);
#5799=VERTEX_POINT('',#30821);
#5800=VERTEX_POINT('',#30827);
#5801=VERTEX_POINT('',#30828);
#5802=VERTEX_POINT('',#30830);
#5803=VERTEX_POINT('',#30832);
#5804=VERTEX_POINT('',#30836);
#5805=VERTEX_POINT('',#30840);
#5806=VERTEX_POINT('',#30846);
#5807=VERTEX_POINT('',#30847);
#5808=VERTEX_POINT('',#30849);
#5809=VERTEX_POINT('',#30851);
#5810=VERTEX_POINT('',#30855);
#5811=VERTEX_POINT('',#30859);
#5812=VERTEX_POINT('',#30865);
#5813=VERTEX_POINT('',#30866);
#5814=VERTEX_POINT('',#30868);
#5815=VERTEX_POINT('',#30870);
#5816=VERTEX_POINT('',#30874);
#5817=VERTEX_POINT('',#30878);
#5818=VERTEX_POINT('',#30884);
#5819=VERTEX_POINT('',#30886);
#5820=VERTEX_POINT('',#30890);
#5821=VERTEX_POINT('',#30894);
#5822=VERTEX_POINT('',#30897);
#5823=VERTEX_POINT('',#30905);
#5824=VERTEX_POINT('',#30947);
#5825=VERTEX_POINT('',#30953);
#5826=VERTEX_POINT('',#30955);
#5827=VERTEX_POINT('',#30957);
#5828=VERTEX_POINT('',#30961);
#5829=VERTEX_POINT('',#30964);
#5830=VERTEX_POINT('',#30968);
#5831=VERTEX_POINT('',#30970);
#5832=VERTEX_POINT('',#30972);
#5833=VERTEX_POINT('',#30976);
#5834=VERTEX_POINT('',#30977);
#5835=VERTEX_POINT('',#30982);
#5836=VERTEX_POINT('',#30990);
#5837=VERTEX_POINT('',#30991);
#5838=VERTEX_POINT('',#30993);
#5839=VERTEX_POINT('',#31007);
#5840=VERTEX_POINT('',#31008);
#5841=VERTEX_POINT('',#31015);
#5842=VERTEX_POINT('',#31024);
#5843=VERTEX_POINT('',#31025);
#5844=VERTEX_POINT('',#31027);
#5845=VERTEX_POINT('',#31041);
#5846=VERTEX_POINT('',#31042);
#5847=VERTEX_POINT('',#31049);
#5848=VERTEX_POINT('',#31058);
#5849=VERTEX_POINT('',#31059);
#5850=VERTEX_POINT('',#31061);
#5851=VERTEX_POINT('',#31075);
#5852=VERTEX_POINT('',#31076);
#5853=VERTEX_POINT('',#31083);
#5854=VERTEX_POINT('',#31111);
#5855=VERTEX_POINT('',#31112);
#5856=VERTEX_POINT('',#31152);
#5857=VERTEX_POINT('',#31153);
#5858=VERTEX_POINT('',#31179);
#5859=VERTEX_POINT('',#31180);
#5860=VERTEX_POINT('',#31239);
#5861=VERTEX_POINT('',#31240);
#5862=VERTEX_POINT('',#31280);
#5863=VERTEX_POINT('',#31281);
#5864=VERTEX_POINT('',#31288);
#5865=VERTEX_POINT('',#31289);
#5866=VERTEX_POINT('',#31315);
#5867=VERTEX_POINT('',#31316);
#5868=VERTEX_POINT('',#31375);
#5869=VERTEX_POINT('',#31376);
#5870=VERTEX_POINT('',#31390);
#5871=VERTEX_POINT('',#31421);
#5872=VERTEX_POINT('',#31422);
#5873=VERTEX_POINT('',#31429);
#5874=VERTEX_POINT('',#31430);
#5875=VERTEX_POINT('',#31456);
#5876=VERTEX_POINT('',#31457);
#5877=VERTEX_POINT('',#31497);
#5878=VERTEX_POINT('',#31498);
#5879=VERTEX_POINT('',#31517);
#5880=VERTEX_POINT('',#31519);
#5881=VERTEX_POINT('',#31546);
#5882=VERTEX_POINT('',#31550);
#5883=VERTEX_POINT('',#31553);
#5884=VERTEX_POINT('',#31557);
#5885=VERTEX_POINT('',#31561);
#5886=VERTEX_POINT('',#31565);
#5887=VERTEX_POINT('',#31569);
#5888=EDGE_CURVE('',#4682,#4683,#3272,.T.);
#5889=EDGE_CURVE('',#4683,#4684,#3273,.T.);
#5890=EDGE_CURVE('',#4684,#4685,#3274,.T.);
#5891=EDGE_CURVE('',#4685,#4686,#3275,.T.);
#5892=EDGE_CURVE('',#4686,#4687,#3276,.T.);
#5893=EDGE_CURVE('',#4687,#4682,#3277,.T.);
#5894=EDGE_CURVE('',#4688,#4686,#3278,.T.);
#5895=EDGE_CURVE('',#4689,#4688,#1405,.T.);
#5896=EDGE_CURVE('',#4690,#4689,#3279,.T.);
#5897=EDGE_CURVE('',#4691,#4690,#1406,.T.);
#5898=EDGE_CURVE('',#4687,#4691,#3280,.T.);
#5899=EDGE_CURVE('',#4692,#4692,#1407,.T.);
#5900=EDGE_CURVE('',#4685,#4693,#3281,.T.);
#5901=EDGE_CURVE('',#4694,#4693,#3282,.T.);
#5902=EDGE_CURVE('',#4694,#4688,#3283,.T.);
#5903=EDGE_CURVE('',#4695,#4684,#3284,.T.);
#5904=EDGE_CURVE('',#4696,#4695,#3285,.T.);
#5905=EDGE_CURVE('',#4697,#4696,#3286,.T.);
#5906=EDGE_CURVE('',#4698,#4697,#3287,.T.);
#5907=EDGE_CURVE('',#4693,#4698,#3288,.T.);
#5908=EDGE_CURVE('',#4695,#4699,#3289,.T.);
#5909=EDGE_CURVE('',#4699,#4700,#3290,.T.);
#5910=EDGE_CURVE('',#4700,#4701,#3291,.T.);
#5911=EDGE_CURVE('',#4701,#4702,#3292,.T.);
#5912=EDGE_CURVE('',#4702,#4696,#3293,.T.);
#5913=EDGE_CURVE('',#4703,#4701,#3294,.T.);
#5914=EDGE_CURVE('',#4704,#4703,#3295,.T.);
#5915=EDGE_CURVE('',#4702,#4704,#3296,.T.);
#5916=EDGE_CURVE('',#4700,#4705,#3297,.T.);
#5917=EDGE_CURVE('',#4706,#4705,#3298,.T.);
#5918=EDGE_CURVE('',#4706,#4707,#3299,.T.);
#5919=EDGE_CURVE('',#4703,#4707,#3300,.T.);
#5920=EDGE_CURVE('',#4708,#4682,#3301,.T.);
#5921=EDGE_CURVE('',#4709,#4708,#3302,.T.);
#5922=EDGE_CURVE('',#4705,#4709,#3303,.T.);
#5923=EDGE_CURVE('',#4683,#4699,#3304,.T.);
#5924=EDGE_CURVE('',#4707,#4710,#3305,.T.);
#5925=EDGE_CURVE('',#4710,#4711,#3306,.T.);
#5926=EDGE_CURVE('',#4711,#4712,#3307,.T.);
#5927=EDGE_CURVE('',#4712,#4704,#3308,.T.);
#5928=EDGE_CURVE('',#4712,#4713,#3309,.T.);
#5929=EDGE_CURVE('',#4697,#4713,#3310,.T.);
#5930=EDGE_CURVE('',#4714,#4711,#3311,.T.);
#5931=EDGE_CURVE('',#4715,#4714,#3312,.T.);
#5932=EDGE_CURVE('',#4716,#4715,#3313,.T.);
#5933=EDGE_CURVE('',#4717,#4716,#3314,.T.);
#5934=EDGE_CURVE('',#4713,#4717,#3315,.T.);
#5935=EDGE_CURVE('',#4714,#4718,#3316,.T.);
#5936=EDGE_CURVE('',#4718,#4719,#3317,.T.);
#5937=EDGE_CURVE('',#4719,#4720,#3318,.T.);
#5938=EDGE_CURVE('',#4720,#4721,#3319,.T.);
#5939=EDGE_CURVE('',#4721,#4715,#3320,.T.);
#5940=EDGE_CURVE('',#4722,#4720,#3321,.T.);
#5941=EDGE_CURVE('',#4723,#4722,#3322,.T.);
#5942=EDGE_CURVE('',#4721,#4723,#3323,.T.);
#5943=EDGE_CURVE('',#4724,#4724,#1408,.T.);
#5944=EDGE_CURVE('',#4719,#4725,#3324,.T.);
#5945=EDGE_CURVE('',#4726,#4725,#3325,.T.);
#5946=EDGE_CURVE('',#4726,#4727,#3326,.T.);
#5947=EDGE_CURVE('',#4722,#4727,#3327,.T.);
#5948=EDGE_CURVE('',#4728,#4706,#3328,.T.);
#5949=EDGE_CURVE('',#4725,#4728,#3329,.T.);
#5950=EDGE_CURVE('',#4710,#4718,#3330,.T.);
#5951=EDGE_CURVE('',#4727,#4729,#3331,.T.);
#5952=EDGE_CURVE('',#4729,#4730,#3332,.T.);
#5953=EDGE_CURVE('',#4730,#4731,#3333,.T.);
#5954=EDGE_CURVE('',#4731,#4723,#3334,.T.);
#5955=EDGE_CURVE('',#4731,#4732,#3335,.T.);
#5956=EDGE_CURVE('',#4716,#4732,#3336,.T.);
#5957=EDGE_CURVE('',#4733,#4730,#3337,.T.);
#5958=EDGE_CURVE('',#4734,#4733,#3338,.T.);
#5959=EDGE_CURVE('',#4735,#4734,#3339,.T.);
#5960=EDGE_CURVE('',#4736,#4735,#3340,.T.);
#5961=EDGE_CURVE('',#4732,#4736,#3341,.T.);
#5962=EDGE_CURVE('',#4729,#4737,#3342,.T.);
#5963=EDGE_CURVE('',#4733,#4737,#3343,.T.);
#5964=EDGE_CURVE('',#4737,#4738,#3344,.T.);
#5965=EDGE_CURVE('',#4738,#4739,#3345,.T.);
#5966=EDGE_CURVE('',#4739,#4740,#3346,.T.);
#5967=EDGE_CURVE('',#4740,#4734,#3347,.T.);
#5968=EDGE_CURVE('',#4740,#4741,#3348,.T.);
#5969=EDGE_CURVE('',#4742,#4741,#3349,.T.);
#5970=EDGE_CURVE('',#4742,#4743,#3350,.T.);
#5971=EDGE_CURVE('',#4735,#4743,#3351,.T.);
#5972=EDGE_CURVE('',#4744,#4745,#3352,.T.);
#5973=EDGE_CURVE('',#4745,#4746,#3353,.T.);
#5974=EDGE_CURVE('',#4746,#4747,#3354,.T.);
#5975=EDGE_CURVE('',#4747,#4748,#3355,.T.);
#5976=EDGE_CURVE('',#4748,#4749,#3356,.T.);
#5977=EDGE_CURVE('',#4749,#4744,#3357,.T.);
#5978=EDGE_CURVE('',#4750,#4744,#3358,.T.);
#5979=EDGE_CURVE('',#4751,#4750,#3359,.T.);
#5980=EDGE_CURVE('',#4743,#4751,#3360,.T.);
#5981=EDGE_CURVE('',#4752,#4742,#3361,.T.);
#5982=EDGE_CURVE('',#4745,#4752,#3362,.T.);
#5983=EDGE_CURVE('',#4749,#4753,#3363,.T.);
#5984=EDGE_CURVE('',#4754,#4753,#3364,.T.);
#5985=EDGE_CURVE('',#4754,#4755,#3365,.T.);
#5986=EDGE_CURVE('',#4750,#4755,#3366,.T.);
#5987=EDGE_CURVE('',#4756,#4748,#3367,.T.);
#5988=EDGE_CURVE('',#4753,#4756,#3368,.T.);
#5989=EDGE_CURVE('',#4757,#4757,#1409,.T.);
#5990=EDGE_CURVE('',#4758,#4759,#3369,.T.);
#5991=EDGE_CURVE('',#4759,#4752,#3370,.T.);
#5992=EDGE_CURVE('',#4741,#4760,#3371,.T.);
#5993=EDGE_CURVE('',#4760,#4758,#3372,.T.);
#5994=EDGE_CURVE('',#4759,#4746,#3373,.T.);
#5995=EDGE_CURVE('',#4761,#4758,#3374,.T.);
#5996=EDGE_CURVE('',#4762,#4761,#3375,.T.);
#5997=EDGE_CURVE('',#4763,#4762,#3376,.T.);
#5998=EDGE_CURVE('',#4747,#4763,#3377,.T.);
#5999=EDGE_CURVE('',#4738,#4764,#3378,.T.);
#6000=EDGE_CURVE('',#4761,#4764,#3379,.T.);
#6001=EDGE_CURVE('',#4760,#4739,#3380,.T.);
#6002=EDGE_CURVE('',#4765,#4766,#3381,.T.);
#6003=EDGE_CURVE('',#4766,#4767,#3382,.T.);
#6004=EDGE_CURVE('',#4767,#4754,#3383,.T.);
#6005=EDGE_CURVE('',#4756,#4765,#3384,.T.);
#6006=EDGE_CURVE('',#4768,#4767,#3385,.T.);
#6007=EDGE_CURVE('',#4769,#4768,#3386,.T.);
#6008=EDGE_CURVE('',#4770,#4769,#3387,.T.);
#6009=EDGE_CURVE('',#4771,#4770,#3388,.T.);
#6010=EDGE_CURVE('',#4755,#4771,#3389,.T.);
#6011=EDGE_CURVE('',#4768,#4772,#3390,.T.);
#6012=EDGE_CURVE('',#4772,#4773,#3391,.T.);
#6013=EDGE_CURVE('',#4773,#4774,#3392,.T.);
#6014=EDGE_CURVE('',#4774,#4775,#3393,.T.);
#6015=EDGE_CURVE('',#4775,#4769,#3394,.T.);
#6016=EDGE_CURVE('',#4776,#4774,#3395,.T.);
#6017=EDGE_CURVE('',#4777,#4776,#3396,.T.);
#6018=EDGE_CURVE('',#4775,#4777,#3397,.T.);
#6019=EDGE_CURVE('',#4773,#4778,#3398,.T.);
#6020=EDGE_CURVE('',#4779,#4778,#3399,.T.);
#6021=EDGE_CURVE('',#4779,#4780,#3400,.T.);
#6022=EDGE_CURVE('',#4776,#4780,#3401,.T.);
#6023=EDGE_CURVE('',#4781,#4765,#3402,.T.);
#6024=EDGE_CURVE('',#4782,#4781,#3403,.T.);
#6025=EDGE_CURVE('',#4778,#4782,#3404,.T.);
#6026=EDGE_CURVE('',#4766,#4772,#3405,.T.);
#6027=EDGE_CURVE('',#4780,#4783,#3406,.T.);
#6028=EDGE_CURVE('',#4783,#4784,#3407,.T.);
#6029=EDGE_CURVE('',#4784,#4785,#3408,.T.);
#6030=EDGE_CURVE('',#4785,#4777,#3409,.T.);
#6031=EDGE_CURVE('',#4785,#4786,#3410,.T.);
#6032=EDGE_CURVE('',#4770,#4786,#3411,.T.);
#6033=EDGE_CURVE('',#4787,#4784,#3412,.T.);
#6034=EDGE_CURVE('',#4788,#4787,#3413,.T.);
#6035=EDGE_CURVE('',#4789,#4788,#3414,.T.);
#6036=EDGE_CURVE('',#4790,#4789,#3415,.T.);
#6037=EDGE_CURVE('',#4786,#4790,#3416,.T.);
#6038=EDGE_CURVE('',#4787,#4791,#3417,.T.);
#6039=EDGE_CURVE('',#4791,#4792,#3418,.T.);
#6040=EDGE_CURVE('',#4792,#4793,#3419,.T.);
#6041=EDGE_CURVE('',#4793,#4794,#3420,.T.);
#6042=EDGE_CURVE('',#4794,#4788,#3421,.T.);
#6043=EDGE_CURVE('',#4795,#4793,#3422,.T.);
#6044=EDGE_CURVE('',#4796,#4795,#1410,.T.);
#6045=EDGE_CURVE('',#4797,#4796,#3423,.T.);
#6046=EDGE_CURVE('',#4798,#4797,#1411,.T.);
#6047=EDGE_CURVE('',#4794,#4798,#3424,.T.);
#6048=EDGE_CURVE('',#4799,#4799,#1412,.T.);
#6049=EDGE_CURVE('',#4792,#4800,#3425,.T.);
#6050=EDGE_CURVE('',#4801,#4800,#3426,.T.);
#6051=EDGE_CURVE('',#4801,#4795,#3427,.T.);
#6052=EDGE_CURVE('',#4802,#4779,#3428,.T.);
#6053=EDGE_CURVE('',#4800,#4802,#3429,.T.);
#6054=EDGE_CURVE('',#4783,#4791,#3430,.T.);
#6055=EDGE_CURVE('',#4790,#4803,#3431,.T.);
#6056=EDGE_CURVE('',#4803,#4804,#3432,.T.);
#6057=EDGE_CURVE('',#4804,#4771,#3433,.T.);
#6058=EDGE_CURVE('',#4789,#4805,#3434,.T.);
#6059=EDGE_CURVE('',#4806,#4805,#3435,.T.);
#6060=EDGE_CURVE('',#4806,#4803,#3436,.T.);
#6061=EDGE_CURVE('',#4807,#4808,#457,.T.);
#6062=EDGE_CURVE('',#4808,#4806,#458,.T.);
#6063=EDGE_CURVE('',#4805,#4807,#459,.T.);
#6064=EDGE_CURVE('',#4807,#4809,#460,.T.);
#6065=EDGE_CURVE('',#4809,#4808,#461,.T.);
#6066=EDGE_CURVE('',#4810,#4809,#462,.T.);
#6067=EDGE_CURVE('',#4811,#4810,#463,.T.);
#6068=EDGE_CURVE('',#4812,#4811,#3437,.T.);
#6069=EDGE_CURVE('',#4813,#4812,#464,.T.);
#6070=EDGE_CURVE('',#4814,#4813,#465,.T.);
#6071=EDGE_CURVE('',#4815,#4814,#466,.T.);
#6072=EDGE_CURVE('',#4816,#4815,#467,.T.);
#6073=EDGE_CURVE('',#4817,#4816,#3438,.T.);
#6074=EDGE_CURVE('',#4818,#4817,#3439,.T.);
#6075=EDGE_CURVE('',#4819,#4818,#3440,.T.);
#6076=EDGE_CURVE('',#4820,#4819,#3441,.T.);
#6077=EDGE_CURVE('',#4804,#4820,#3442,.T.);
#6078=EDGE_CURVE('',#4821,#4821,#1413,.T.);
#6079=EDGE_CURVE('',#4822,#4822,#1414,.T.);
#6080=EDGE_CURVE('',#4823,#4823,#1415,.T.);
#6081=EDGE_CURVE('',#4824,#4824,#1416,.T.);
#6082=EDGE_CURVE('',#4798,#4805,#3443,.T.);
#6083=EDGE_CURVE('',#4798,#4825,#468,.T.);
#6084=EDGE_CURVE('',#4809,#4825,#3444,.T.);
#6085=EDGE_CURVE('',#4751,#4820,#3445,.T.);
#6086=EDGE_CURVE('',#4819,#4736,#3446,.T.);
#6087=EDGE_CURVE('',#4717,#4818,#3447,.T.);
#6088=EDGE_CURVE('',#4817,#4698,#3448,.T.);
#6089=EDGE_CURVE('',#4816,#4694,#3449,.T.);
#6090=EDGE_CURVE('',#4815,#4826,#469,.T.);
#6091=EDGE_CURVE('',#4826,#4694,#470,.T.);
#6092=EDGE_CURVE('',#4814,#4826,#471,.T.);
#6093=EDGE_CURVE('',#4709,#4827,#3450,.T.);
#6094=EDGE_CURVE('',#4827,#4828,#3451,.T.);
#6095=EDGE_CURVE('',#4828,#4728,#3452,.T.);
#6096=EDGE_CURVE('',#4708,#4829,#3453,.T.);
#6097=EDGE_CURVE('',#4830,#4829,#3454,.T.);
#6098=EDGE_CURVE('',#4830,#4827,#3455,.T.);
#6099=EDGE_CURVE('',#4831,#4832,#472,.T.);
#6100=EDGE_CURVE('',#4832,#4830,#473,.T.);
#6101=EDGE_CURVE('',#4829,#4831,#474,.T.);
#6102=EDGE_CURVE('',#4831,#4833,#475,.T.);
#6103=EDGE_CURVE('',#4833,#4832,#476,.T.);
#6104=EDGE_CURVE('',#4834,#4833,#477,.T.);
#6105=EDGE_CURVE('',#4835,#4834,#478,.T.);
#6106=EDGE_CURVE('',#4836,#4835,#3456,.T.);
#6107=EDGE_CURVE('',#4837,#4836,#479,.T.);
#6108=EDGE_CURVE('',#4838,#4837,#480,.T.);
#6109=EDGE_CURVE('',#4839,#4838,#481,.T.);
#6110=EDGE_CURVE('',#4840,#4839,#482,.T.);
#6111=EDGE_CURVE('',#4841,#4840,#3457,.T.);
#6112=EDGE_CURVE('',#4842,#4841,#3458,.T.);
#6113=EDGE_CURVE('',#4843,#4842,#3459,.T.);
#6114=EDGE_CURVE('',#4844,#4843,#3460,.T.);
#6115=EDGE_CURVE('',#4828,#4844,#3461,.T.);
#6116=EDGE_CURVE('',#4845,#4845,#1417,.T.);
#6117=EDGE_CURVE('',#4846,#4846,#1418,.T.);
#6118=EDGE_CURVE('',#4847,#4847,#1419,.T.);
#6119=EDGE_CURVE('',#4848,#4848,#1420,.T.);
#6120=EDGE_CURVE('',#4691,#4829,#3462,.T.);
#6121=EDGE_CURVE('',#4691,#4849,#483,.T.);
#6122=EDGE_CURVE('',#4833,#4849,#3463,.T.);
#6123=EDGE_CURVE('',#4764,#4850,#3464,.T.);
#6124=EDGE_CURVE('',#4850,#4844,#3465,.T.);
#6125=EDGE_CURVE('',#4843,#4762,#3466,.T.);
#6126=EDGE_CURVE('',#4850,#4726,#3467,.T.);
#6127=EDGE_CURVE('',#4782,#4842,#3468,.T.);
#6128=EDGE_CURVE('',#4841,#4802,#3469,.T.);
#6129=EDGE_CURVE('',#4781,#4763,#3470,.T.);
#6130=EDGE_CURVE('',#4840,#4801,#3471,.T.);
#6131=EDGE_CURVE('',#4839,#4851,#484,.T.);
#6132=EDGE_CURVE('',#4851,#4801,#485,.T.);
#6133=EDGE_CURVE('',#4838,#4851,#486,.T.);
#6134=EDGE_CURVE('',#4848,#4852,#3472,.T.);
#6135=EDGE_CURVE('',#4852,#4852,#1421,.T.);
#6136=EDGE_CURVE('',#4853,#4853,#1422,.T.);
#6137=EDGE_CURVE('',#4853,#4852,#3473,.T.);
#6138=EDGE_CURVE('',#4824,#4853,#3474,.T.);
#6139=EDGE_CURVE('',#4845,#4854,#3475,.T.);
#6140=EDGE_CURVE('',#4854,#4854,#1423,.T.);
#6141=EDGE_CURVE('',#4855,#4855,#1424,.T.);
#6142=EDGE_CURVE('',#4855,#4854,#3476,.T.);
#6143=EDGE_CURVE('',#4821,#4855,#3477,.T.);
#6144=EDGE_CURVE('',#4847,#4856,#3478,.T.);
#6145=EDGE_CURVE('',#4856,#4856,#1425,.T.);
#6146=EDGE_CURVE('',#4857,#4857,#1426,.T.);
#6147=EDGE_CURVE('',#4857,#4856,#3479,.T.);
#6148=EDGE_CURVE('',#4823,#4857,#3480,.T.);
#6149=EDGE_CURVE('',#4846,#4858,#3481,.T.);
#6150=EDGE_CURVE('',#4858,#4858,#1427,.T.);
#6151=EDGE_CURVE('',#4859,#4859,#1428,.T.);
#6152=EDGE_CURVE('',#4859,#4858,#3482,.T.);
#6153=EDGE_CURVE('',#4822,#4859,#3483,.T.);
#6154=EDGE_CURVE('',#4860,#4860,#1429,.T.);
#6155=EDGE_CURVE('',#4860,#4861,#3484,.T.);
#6156=EDGE_CURVE('',#4861,#4861,#1430,.T.);
#6157=EDGE_CURVE('',#4861,#4862,#3485,.T.);
#6158=EDGE_CURVE('',#4862,#4862,#1431,.T.);
#6159=EDGE_CURVE('',#4863,#4863,#1432,.T.);
#6160=EDGE_CURVE('',#4863,#4864,#3486,.T.);
#6161=EDGE_CURVE('',#4864,#4864,#1433,.T.);
#6162=EDGE_CURVE('',#4865,#4865,#1434,.T.);
#6163=EDGE_CURVE('',#4865,#4866,#3487,.T.);
#6164=EDGE_CURVE('',#4866,#4866,#1435,.T.);
#6165=EDGE_CURVE('',#4866,#4867,#3488,.T.);
#6166=EDGE_CURVE('',#4867,#4867,#1436,.T.);
#6167=EDGE_CURVE('',#4799,#4868,#3489,.T.);
#6168=EDGE_CURVE('',#4868,#4868,#1437,.T.);
#6169=EDGE_CURVE('',#4868,#4869,#3490,.T.);
#6170=EDGE_CURVE('',#4869,#4869,#1438,.T.);
#6171=EDGE_CURVE('',#4870,#4870,#1439,.T.);
#6172=EDGE_CURVE('',#4870,#4871,#3491,.T.);
#6173=EDGE_CURVE('',#4871,#4871,#1440,.T.);
#6174=EDGE_CURVE('',#4872,#4872,#1441,.T.);
#6175=EDGE_CURVE('',#4872,#4873,#3492,.T.);
#6176=EDGE_CURVE('',#4873,#4873,#1442,.T.);
#6177=EDGE_CURVE('',#4873,#4757,#3493,.T.);
#6178=EDGE_CURVE('',#4724,#4874,#3494,.T.);
#6179=EDGE_CURVE('',#4874,#4874,#1443,.T.);
#6180=EDGE_CURVE('',#4874,#4875,#3495,.T.);
#6181=EDGE_CURVE('',#4875,#4875,#1444,.T.);
#6182=EDGE_CURVE('',#4876,#4876,#1445,.T.);
#6183=EDGE_CURVE('',#4876,#4877,#3496,.T.);
#6184=EDGE_CURVE('',#4877,#4877,#1446,.T.);
#6185=EDGE_CURVE('',#4878,#4878,#1447,.T.);
#6186=EDGE_CURVE('',#4878,#4879,#3497,.T.);
#6187=EDGE_CURVE('',#4879,#4879,#1448,.T.);
#6188=EDGE_CURVE('',#4879,#4692,#3498,.T.);
#6189=EDGE_CURVE('',#4880,#4810,#487,.T.);
#6190=EDGE_CURVE('',#4825,#4880,#488,.T.);
#6191=EDGE_CURVE('',#4881,#4834,#489,.T.);
#6192=EDGE_CURVE('',#4849,#4881,#490,.T.);
#6193=EDGE_CURVE('',#4813,#4882,#491,.T.);
#6194=EDGE_CURVE('',#4882,#4883,#492,.T.);
#6195=EDGE_CURVE('',#4883,#4814,#3499,.T.);
#6196=EDGE_CURVE('',#4883,#4688,#493,.T.);
#6197=EDGE_CURVE('',#4837,#4884,#494,.T.);
#6198=EDGE_CURVE('',#4884,#4885,#495,.T.);
#6199=EDGE_CURVE('',#4885,#4838,#3500,.T.);
#6200=EDGE_CURVE('',#4885,#4795,#496,.T.);
#6201=EDGE_CURVE('',#4880,#4811,#497,.T.);
#6202=EDGE_CURVE('',#4881,#4835,#498,.T.);
#6203=EDGE_CURVE('',#4812,#4882,#499,.T.);
#6204=EDGE_CURVE('',#4836,#4884,#500,.T.);
#6205=EDGE_CURVE('',#4797,#4886,#1449,.T.);
#6206=EDGE_CURVE('',#4886,#4811,#1450,.T.);
#6207=EDGE_CURVE('',#4836,#4887,#1451,.T.);
#6208=EDGE_CURVE('',#4796,#4887,#1452,.T.);
#6209=EDGE_CURVE('',#4690,#4888,#1453,.T.);
#6210=EDGE_CURVE('',#4888,#4835,#1454,.T.);
#6211=EDGE_CURVE('',#4689,#4889,#1455,.T.);
#6212=EDGE_CURVE('',#4889,#4888,#3501,.T.);
#6213=EDGE_CURVE('',#4812,#4889,#1456,.T.);
#6214=EDGE_CURVE('',#4887,#4886,#3502,.T.);
#6215=EDGE_CURVE('',#4888,#4887,#3503,.T.);
#6216=EDGE_CURVE('',#4886,#4889,#3504,.T.);
#6217=EDGE_CURVE('',#4890,#4890,#1457,.T.);
#6218=EDGE_CURVE('',#4890,#4891,#3505,.T.);
#6219=EDGE_CURVE('',#4891,#4892,#1458,.T.);
#6220=EDGE_CURVE('',#4892,#4891,#1459,.T.);
#6221=EDGE_CURVE('',#4892,#4893,#3506,.T.);
#6222=EDGE_CURVE('',#4893,#4894,#501,.T.);
#6223=EDGE_CURVE('',#4894,#4895,#502,.T.);
#6224=EDGE_CURVE('',#4895,#4896,#503,.T.);
#6225=EDGE_CURVE('',#4896,#4897,#1460,.T.);
#6226=EDGE_CURVE('',#4897,#4898,#504,.T.);
#6227=EDGE_CURVE('',#4898,#4899,#505,.T.);
#6228=EDGE_CURVE('',#4899,#4900,#506,.T.);
#6229=EDGE_CURVE('',#4900,#4901,#1461,.T.);
#6230=EDGE_CURVE('',#4901,#4902,#507,.T.);
#6231=EDGE_CURVE('',#4902,#4903,#508,.T.);
#6232=EDGE_CURVE('',#4903,#4904,#509,.T.);
#6233=EDGE_CURVE('',#4904,#4905,#1462,.T.);
#6234=EDGE_CURVE('',#4905,#4906,#510,.T.);
#6235=EDGE_CURVE('',#4906,#4907,#511,.T.);
#6236=EDGE_CURVE('',#4907,#4908,#512,.T.);
#6237=EDGE_CURVE('',#4908,#4909,#1463,.T.);
#6238=EDGE_CURVE('',#4909,#4910,#513,.T.);
#6239=EDGE_CURVE('',#4910,#4911,#514,.T.);
#6240=EDGE_CURVE('',#4911,#4912,#515,.T.);
#6241=EDGE_CURVE('',#4912,#4913,#1464,.T.);
#6242=EDGE_CURVE('',#4913,#4914,#516,.T.);
#6243=EDGE_CURVE('',#4914,#4915,#517,.T.);
#6244=EDGE_CURVE('',#4915,#4916,#518,.T.);
#6245=EDGE_CURVE('',#4916,#4917,#1465,.T.);
#6246=EDGE_CURVE('',#4917,#4918,#519,.T.);
#6247=EDGE_CURVE('',#4918,#4919,#520,.T.);
#6248=EDGE_CURVE('',#4919,#4920,#521,.T.);
#6249=EDGE_CURVE('',#4920,#4921,#1466,.T.);
#6250=EDGE_CURVE('',#4921,#4922,#522,.T.);
#6251=EDGE_CURVE('',#4922,#4923,#523,.T.);
#6252=EDGE_CURVE('',#4923,#4924,#524,.T.);
#6253=EDGE_CURVE('',#4924,#4925,#1467,.T.);
#6254=EDGE_CURVE('',#4925,#4926,#525,.T.);
#6255=EDGE_CURVE('',#4926,#4927,#526,.T.);
#6256=EDGE_CURVE('',#4927,#4928,#527,.T.);
#6257=EDGE_CURVE('',#4928,#4929,#1468,.T.);
#6258=EDGE_CURVE('',#4929,#4930,#528,.T.);
#6259=EDGE_CURVE('',#4930,#4931,#529,.T.);
#6260=EDGE_CURVE('',#4931,#4932,#530,.T.);
#6261=EDGE_CURVE('',#4932,#4933,#1469,.T.);
#6262=EDGE_CURVE('',#4933,#4934,#531,.T.);
#6263=EDGE_CURVE('',#4934,#4935,#532,.T.);
#6264=EDGE_CURVE('',#4935,#4936,#533,.T.);
#6265=EDGE_CURVE('',#4936,#4937,#1470,.T.);
#6266=EDGE_CURVE('',#4937,#4938,#534,.T.);
#6267=EDGE_CURVE('',#4938,#4939,#535,.T.);
#6268=EDGE_CURVE('',#4939,#4940,#536,.T.);
#6269=EDGE_CURVE('',#4940,#4941,#1471,.T.);
#6270=EDGE_CURVE('',#4941,#4942,#537,.T.);
#6271=EDGE_CURVE('',#4942,#4943,#538,.T.);
#6272=EDGE_CURVE('',#4943,#4944,#539,.T.);
#6273=EDGE_CURVE('',#4944,#4945,#1472,.T.);
#6274=EDGE_CURVE('',#4945,#4946,#540,.T.);
#6275=EDGE_CURVE('',#4946,#4947,#541,.T.);
#6276=EDGE_CURVE('',#4947,#4948,#542,.T.);
#6277=EDGE_CURVE('',#4948,#4949,#1473,.T.);
#6278=EDGE_CURVE('',#4949,#4950,#543,.T.);
#6279=EDGE_CURVE('',#4950,#4951,#544,.T.);
#6280=EDGE_CURVE('',#4951,#4952,#545,.T.);
#6281=EDGE_CURVE('',#4952,#4953,#1474,.T.);
#6282=EDGE_CURVE('',#4953,#4954,#546,.T.);
#6283=EDGE_CURVE('',#4954,#4955,#547,.T.);
#6284=EDGE_CURVE('',#4955,#4956,#548,.T.);
#6285=EDGE_CURVE('',#4956,#4957,#1475,.T.);
#6286=EDGE_CURVE('',#4957,#4958,#549,.T.);
#6287=EDGE_CURVE('',#4958,#4959,#550,.T.);
#6288=EDGE_CURVE('',#4959,#4960,#551,.T.);
#6289=EDGE_CURVE('',#4960,#4961,#1476,.T.);
#6290=EDGE_CURVE('',#4961,#4962,#552,.T.);
#6291=EDGE_CURVE('',#4962,#4963,#553,.T.);
#6292=EDGE_CURVE('',#4963,#4964,#554,.T.);
#6293=EDGE_CURVE('',#4964,#4965,#1477,.T.);
#6294=EDGE_CURVE('',#4965,#4966,#555,.T.);
#6295=EDGE_CURVE('',#4966,#4967,#556,.T.);
#6296=EDGE_CURVE('',#4967,#4968,#557,.T.);
#6297=EDGE_CURVE('',#4968,#4969,#1478,.T.);
#6298=EDGE_CURVE('',#4969,#4970,#558,.T.);
#6299=EDGE_CURVE('',#4970,#4971,#559,.T.);
#6300=EDGE_CURVE('',#4971,#4972,#560,.T.);
#6301=EDGE_CURVE('',#4972,#4973,#1479,.T.);
#6302=EDGE_CURVE('',#4973,#4893,#561,.T.);
#6303=EDGE_CURVE('',#4974,#4975,#1480,.T.);
#6304=EDGE_CURVE('',#4974,#4976,#562,.T.);
#6305=EDGE_CURVE('',#4977,#4976,#1481,.T.);
#6306=EDGE_CURVE('',#4977,#4975,#563,.T.);
#6307=EDGE_CURVE('',#4977,#4978,#564,.T.);
#6308=EDGE_CURVE('',#4978,#4979,#565,.T.);
#6309=EDGE_CURVE('',#4979,#4980,#566,.T.);
#6310=EDGE_CURVE('',#4980,#4981,#567,.T.);
#6311=EDGE_CURVE('',#4981,#4980,#568,.T.);
#6312=EDGE_CURVE('',#4979,#4982,#569,.T.);
#6313=EDGE_CURVE('',#4982,#4975,#570,.T.);
#6314=EDGE_CURVE('',#4983,#4982,#1482,.T.);
#6315=EDGE_CURVE('',#4984,#4983,#1483,.T.);
#6316=EDGE_CURVE('',#4974,#4984,#571,.T.);
#6317=EDGE_CURVE('',#4985,#4976,#572,.T.);
#6318=EDGE_CURVE('',#4978,#4985,#1484,.T.);
#6319=EDGE_CURVE('',#4981,#4986,#3507,.T.);
#6320=EDGE_CURVE('',#4987,#4986,#573,.T.);
#6321=EDGE_CURVE('',#4986,#4987,#574,.T.);
#6322=EDGE_CURVE('',#4984,#4988,#575,.T.);
#6323=EDGE_CURVE('',#4988,#4989,#576,.T.);
#6324=EDGE_CURVE('',#4989,#4990,#577,.T.);
#6325=EDGE_CURVE('',#4990,#4989,#578,.T.);
#6326=EDGE_CURVE('',#4988,#4985,#579,.T.);
#6327=EDGE_CURVE('',#4991,#4992,#580,.T.);
#6328=EDGE_CURVE('',#4992,#4991,#581,.T.);
#6329=EDGE_CURVE('',#4992,#4990,#3508,.T.);
#6330=EDGE_CURVE('',#4993,#4993,#1485,.T.);
#6331=EDGE_CURVE('',#4993,#4983,#3509,.T.);
#6332=EDGE_CURVE('',#4994,#4995,#582,.T.);
#6333=EDGE_CURVE('',#4994,#4926,#583,.T.);
#6334=EDGE_CURVE('',#4995,#4925,#584,.T.);
#6335=EDGE_CURVE('',#4996,#4997,#585,.T.);
#6336=EDGE_CURVE('',#4928,#4996,#586,.T.);
#6337=EDGE_CURVE('',#4997,#4927,#587,.T.);
#6338=EDGE_CURVE('',#4997,#4994,#588,.T.);
#6339=EDGE_CURVE('',#4996,#4998,#1486,.T.);
#6340=EDGE_CURVE('',#4998,#4929,#589,.T.);
#6341=EDGE_CURVE('',#4924,#4999,#590,.T.);
#6342=EDGE_CURVE('',#4999,#4995,#1487,.T.);
#6343=EDGE_CURVE('',#5000,#5001,#591,.T.);
#6344=EDGE_CURVE('',#5000,#4922,#592,.T.);
#6345=EDGE_CURVE('',#5001,#4921,#593,.T.);
#6346=EDGE_CURVE('',#4999,#5002,#594,.T.);
#6347=EDGE_CURVE('',#5002,#4923,#595,.T.);
#6348=EDGE_CURVE('',#5002,#5000,#596,.T.);
#6349=EDGE_CURVE('',#4920,#5003,#597,.T.);
#6350=EDGE_CURVE('',#5003,#5001,#1488,.T.);
#6351=EDGE_CURVE('',#5004,#5005,#598,.T.);
#6352=EDGE_CURVE('',#5004,#4918,#599,.T.);
#6353=EDGE_CURVE('',#5005,#4917,#600,.T.);
#6354=EDGE_CURVE('',#5003,#5006,#601,.T.);
#6355=EDGE_CURVE('',#5006,#4919,#602,.T.);
#6356=EDGE_CURVE('',#5006,#5004,#603,.T.);
#6357=EDGE_CURVE('',#4916,#5007,#604,.T.);
#6358=EDGE_CURVE('',#5007,#5005,#1489,.T.);
#6359=EDGE_CURVE('',#5008,#5009,#605,.T.);
#6360=EDGE_CURVE('',#5008,#4914,#606,.T.);
#6361=EDGE_CURVE('',#5009,#4913,#607,.T.);
#6362=EDGE_CURVE('',#5007,#5010,#608,.T.);
#6363=EDGE_CURVE('',#5010,#4915,#609,.T.);
#6364=EDGE_CURVE('',#5010,#5008,#610,.T.);
#6365=EDGE_CURVE('',#4912,#5011,#611,.T.);
#6366=EDGE_CURVE('',#5011,#5009,#1490,.T.);
#6367=EDGE_CURVE('',#5012,#5013,#612,.T.);
#6368=EDGE_CURVE('',#5012,#4910,#613,.T.);
#6369=EDGE_CURVE('',#5013,#4909,#614,.T.);
#6370=EDGE_CURVE('',#5011,#5014,#615,.T.);
#6371=EDGE_CURVE('',#5014,#4911,#616,.T.);
#6372=EDGE_CURVE('',#5014,#5012,#617,.T.);
#6373=EDGE_CURVE('',#4908,#5015,#618,.T.);
#6374=EDGE_CURVE('',#5015,#5013,#1491,.T.);
#6375=EDGE_CURVE('',#5016,#5017,#619,.T.);
#6376=EDGE_CURVE('',#5016,#4906,#620,.T.);
#6377=EDGE_CURVE('',#5017,#4905,#621,.T.);
#6378=EDGE_CURVE('',#5015,#5018,#622,.T.);
#6379=EDGE_CURVE('',#5018,#4907,#623,.T.);
#6380=EDGE_CURVE('',#5018,#5016,#624,.T.);
#6381=EDGE_CURVE('',#4904,#5019,#625,.T.);
#6382=EDGE_CURVE('',#5019,#5017,#1492,.T.);
#6383=EDGE_CURVE('',#5020,#5021,#626,.T.);
#6384=EDGE_CURVE('',#5020,#4902,#627,.T.);
#6385=EDGE_CURVE('',#5021,#4901,#628,.T.);
#6386=EDGE_CURVE('',#5019,#5022,#629,.T.);
#6387=EDGE_CURVE('',#5022,#4903,#630,.T.);
#6388=EDGE_CURVE('',#5022,#5020,#631,.T.);
#6389=EDGE_CURVE('',#4900,#5023,#632,.T.);
#6390=EDGE_CURVE('',#5023,#5021,#1493,.T.);
#6391=EDGE_CURVE('',#5024,#5025,#633,.T.);
#6392=EDGE_CURVE('',#5024,#4898,#634,.T.);
#6393=EDGE_CURVE('',#5025,#4897,#635,.T.);
#6394=EDGE_CURVE('',#5023,#5026,#636,.T.);
#6395=EDGE_CURVE('',#5026,#4899,#637,.T.);
#6396=EDGE_CURVE('',#5026,#5024,#638,.T.);
#6397=EDGE_CURVE('',#4896,#5027,#639,.T.);
#6398=EDGE_CURVE('',#5027,#5025,#1494,.T.);
#6399=EDGE_CURVE('',#5028,#5029,#640,.T.);
#6400=EDGE_CURVE('',#5028,#4894,#641,.T.);
#6401=EDGE_CURVE('',#5029,#4973,#642,.T.);
#6402=EDGE_CURVE('',#5027,#5030,#643,.T.);
#6403=EDGE_CURVE('',#5030,#4895,#644,.T.);
#6404=EDGE_CURVE('',#5030,#5028,#645,.T.);
#6405=EDGE_CURVE('',#4972,#5031,#646,.T.);
#6406=EDGE_CURVE('',#5031,#5029,#1495,.T.);
#6407=EDGE_CURVE('',#5032,#5033,#647,.T.);
#6408=EDGE_CURVE('',#5032,#4970,#648,.T.);
#6409=EDGE_CURVE('',#5034,#4969,#649,.T.);
#6410=EDGE_CURVE('',#5033,#5034,#650,.T.);
#6411=EDGE_CURVE('',#5031,#5035,#651,.T.);
#6412=EDGE_CURVE('',#5035,#4971,#652,.T.);
#6413=EDGE_CURVE('',#5035,#5032,#653,.T.);
#6414=EDGE_CURVE('',#4968,#5036,#654,.T.);
#6415=EDGE_CURVE('',#5036,#5034,#1496,.T.);
#6416=EDGE_CURVE('',#5037,#5038,#655,.T.);
#6417=EDGE_CURVE('',#5037,#4966,#656,.T.);
#6418=EDGE_CURVE('',#5038,#4965,#657,.T.);
#6419=EDGE_CURVE('',#5036,#5039,#658,.T.);
#6420=EDGE_CURVE('',#5039,#4967,#659,.T.);
#6421=EDGE_CURVE('',#5039,#5037,#660,.T.);
#6422=EDGE_CURVE('',#4964,#5040,#661,.T.);
#6423=EDGE_CURVE('',#5040,#5038,#1497,.T.);
#6424=EDGE_CURVE('',#5041,#5042,#662,.T.);
#6425=EDGE_CURVE('',#5041,#4962,#663,.T.);
#6426=EDGE_CURVE('',#5042,#4961,#664,.T.);
#6427=EDGE_CURVE('',#5040,#5043,#665,.T.);
#6428=EDGE_CURVE('',#5043,#4963,#666,.T.);
#6429=EDGE_CURVE('',#5043,#5041,#667,.T.);
#6430=EDGE_CURVE('',#4960,#5044,#668,.T.);
#6431=EDGE_CURVE('',#5044,#5042,#1498,.T.);
#6432=EDGE_CURVE('',#5045,#5046,#669,.T.);
#6433=EDGE_CURVE('',#5045,#4958,#670,.T.);
#6434=EDGE_CURVE('',#5046,#4957,#671,.T.);
#6435=EDGE_CURVE('',#5044,#5047,#672,.T.);
#6436=EDGE_CURVE('',#5047,#4959,#673,.T.);
#6437=EDGE_CURVE('',#5047,#5045,#674,.T.);
#6438=EDGE_CURVE('',#4956,#5048,#675,.T.);
#6439=EDGE_CURVE('',#5048,#5046,#1499,.T.);
#6440=EDGE_CURVE('',#5049,#5050,#676,.T.);
#6441=EDGE_CURVE('',#5049,#4954,#677,.T.);
#6442=EDGE_CURVE('',#5050,#4953,#678,.T.);
#6443=EDGE_CURVE('',#5048,#5051,#679,.T.);
#6444=EDGE_CURVE('',#5051,#4955,#680,.T.);
#6445=EDGE_CURVE('',#5051,#5049,#681,.T.);
#6446=EDGE_CURVE('',#4952,#5052,#682,.T.);
#6447=EDGE_CURVE('',#5052,#5050,#1500,.T.);
#6448=EDGE_CURVE('',#5053,#5054,#683,.T.);
#6449=EDGE_CURVE('',#5053,#4950,#684,.T.);
#6450=EDGE_CURVE('',#5054,#4949,#685,.T.);
#6451=EDGE_CURVE('',#5052,#5055,#686,.T.);
#6452=EDGE_CURVE('',#5055,#4951,#687,.T.);
#6453=EDGE_CURVE('',#5055,#5053,#688,.T.);
#6454=EDGE_CURVE('',#4948,#5056,#689,.T.);
#6455=EDGE_CURVE('',#5056,#5054,#1501,.T.);
#6456=EDGE_CURVE('',#5057,#5058,#690,.T.);
#6457=EDGE_CURVE('',#5057,#4946,#691,.T.);
#6458=EDGE_CURVE('',#5058,#4945,#692,.T.);
#6459=EDGE_CURVE('',#5056,#5059,#693,.T.);
#6460=EDGE_CURVE('',#5059,#4947,#694,.T.);
#6461=EDGE_CURVE('',#5059,#5057,#695,.T.);
#6462=EDGE_CURVE('',#4944,#5060,#696,.T.);
#6463=EDGE_CURVE('',#5060,#5058,#1502,.T.);
#6464=EDGE_CURVE('',#5061,#5062,#697,.T.);
#6465=EDGE_CURVE('',#5061,#4942,#698,.T.);
#6466=EDGE_CURVE('',#5062,#4941,#699,.T.);
#6467=EDGE_CURVE('',#5060,#5063,#700,.T.);
#6468=EDGE_CURVE('',#5063,#4943,#701,.T.);
#6469=EDGE_CURVE('',#5063,#5061,#702,.T.);
#6470=EDGE_CURVE('',#4940,#5064,#703,.T.);
#6471=EDGE_CURVE('',#5064,#5062,#1503,.T.);
#6472=EDGE_CURVE('',#5065,#5066,#704,.T.);
#6473=EDGE_CURVE('',#5065,#4938,#705,.T.);
#6474=EDGE_CURVE('',#5066,#4937,#706,.T.);
#6475=EDGE_CURVE('',#5064,#5067,#707,.T.);
#6476=EDGE_CURVE('',#5067,#4939,#708,.T.);
#6477=EDGE_CURVE('',#5067,#5065,#709,.T.);
#6478=EDGE_CURVE('',#4936,#5068,#710,.T.);
#6479=EDGE_CURVE('',#5068,#5066,#1504,.T.);
#6480=EDGE_CURVE('',#5069,#4935,#711,.T.);
#6481=EDGE_CURVE('',#5068,#5069,#712,.T.);
#6482=EDGE_CURVE('',#5070,#4934,#713,.T.);
#6483=EDGE_CURVE('',#5069,#5070,#714,.T.);
#6484=EDGE_CURVE('',#5071,#4933,#715,.T.);
#6485=EDGE_CURVE('',#5070,#5071,#716,.T.);
#6486=EDGE_CURVE('',#5072,#4931,#717,.T.);
#6487=EDGE_CURVE('',#5073,#5072,#718,.T.);
#6488=EDGE_CURVE('',#4932,#5073,#719,.T.);
#6489=EDGE_CURVE('',#5074,#4930,#720,.T.);
#6490=EDGE_CURVE('',#5072,#5074,#721,.T.);
#6491=EDGE_CURVE('',#5074,#4998,#722,.T.);
#6492=EDGE_CURVE('',#5075,#5075,#1505,.T.);
#6493=EDGE_CURVE('',#5075,#5033,#3510,.T.);
#6494=EDGE_CURVE('',#5073,#5071,#1506,.T.);
#6495=EDGE_CURVE('',#5076,#5076,#1507,.T.);
#6496=EDGE_CURVE('',#5076,#5077,#3511,.T.);
#6497=EDGE_CURVE('',#5077,#5077,#1508,.T.);
#6498=EDGE_CURVE('',#5077,#5078,#3512,.T.);
#6499=EDGE_CURVE('',#5078,#5078,#1509,.T.);
#6500=EDGE_CURVE('',#5078,#5079,#3513,.T.);
#6501=EDGE_CURVE('',#5079,#5079,#1510,.T.);
#6502=EDGE_CURVE('',#5080,#5080,#1511,.T.);
#6503=EDGE_CURVE('',#5080,#5081,#3514,.T.);
#6504=EDGE_CURVE('',#5081,#5082,#1512,.T.);
#6505=EDGE_CURVE('',#5082,#5081,#1513,.T.);
#6506=EDGE_CURVE('',#5083,#5083,#1514,.T.);
#6507=EDGE_CURVE('',#5083,#5082,#3515,.T.);
#6508=EDGE_CURVE('',#5084,#5084,#1515,.T.);
#6509=EDGE_CURVE('',#5085,#5083,#3516,.T.);
#6510=EDGE_CURVE('',#5086,#5087,#1516,.T.);
#6511=EDGE_CURVE('',#5086,#5087,#3517,.T.);
#6512=EDGE_CURVE('',#5088,#5089,#1517,.T.);
#6513=EDGE_CURVE('',#5088,#5089,#3518,.T.);
#6514=EDGE_CURVE('',#5089,#5086,#3519,.T.);
#6515=EDGE_CURVE('',#5087,#5088,#3520,.T.);
#6516=EDGE_CURVE('',#5090,#5091,#1518,.T.);
#6517=EDGE_CURVE('',#5091,#5090,#3521,.T.);
#6518=EDGE_CURVE('',#5092,#5090,#3522,.T.);
#6519=EDGE_CURVE('',#5092,#5093,#3523,.T.);
#6520=EDGE_CURVE('',#5091,#5093,#3524,.T.);
#6521=EDGE_CURVE('',#5093,#5092,#1519,.T.);
#6522=EDGE_CURVE('',#5094,#5094,#1520,.T.);
#6523=EDGE_CURVE('',#5095,#5095,#1521,.T.);
#6524=EDGE_CURVE('',#5095,#5094,#3525,.T.);
#6525=EDGE_CURVE('',#5096,#5096,#1522,.T.);
#6526=EDGE_CURVE('',#5096,#5095,#3526,.T.);
#6527=EDGE_CURVE('',#5097,#5097,#1523,.T.);
#6528=EDGE_CURVE('',#5098,#5098,#1524,.T.);
#6529=EDGE_CURVE('',#5098,#5097,#3527,.T.);
#6530=EDGE_CURVE('',#5099,#5099,#1525,.T.);
#6531=EDGE_CURVE('',#5100,#5100,#1526,.T.);
#6532=EDGE_CURVE('',#5100,#5099,#3528,.T.);
#6533=EDGE_CURVE('',#5084,#5100,#3529,.T.);
#6534=EDGE_CURVE('',#5101,#5102,#723,.T.);
#6535=EDGE_CURVE('',#5101,#5103,#724,.T.);
#6536=EDGE_CURVE('',#5103,#5104,#725,.T.);
#6537=EDGE_CURVE('',#5104,#5105,#726,.T.);
#6538=EDGE_CURVE('',#5105,#5106,#727,.T.);
#6539=EDGE_CURVE('',#5106,#5105,#728,.T.);
#6540=EDGE_CURVE('',#5104,#5107,#729,.T.);
#6541=EDGE_CURVE('',#5107,#5102,#730,.T.);
#6542=EDGE_CURVE('',#5108,#5107,#1527,.T.);
#6543=EDGE_CURVE('',#5109,#5108,#1528,.T.);
#6544=EDGE_CURVE('',#5110,#5109,#731,.T.);
#6545=EDGE_CURVE('',#5110,#5102,#1529,.T.);
#6546=EDGE_CURVE('',#5101,#5111,#1530,.T.);
#6547=EDGE_CURVE('',#5112,#5111,#732,.T.);
#6548=EDGE_CURVE('',#5103,#5112,#1531,.T.);
#6549=EDGE_CURVE('',#5106,#5113,#3530,.T.);
#6550=EDGE_CURVE('',#5114,#5113,#733,.T.);
#6551=EDGE_CURVE('',#5113,#5114,#734,.T.);
#6552=EDGE_CURVE('',#5110,#5111,#735,.T.);
#6553=EDGE_CURVE('',#5109,#5115,#736,.T.);
#6554=EDGE_CURVE('',#5115,#5116,#737,.T.);
#6555=EDGE_CURVE('',#5116,#5117,#738,.T.);
#6556=EDGE_CURVE('',#5117,#5116,#739,.T.);
#6557=EDGE_CURVE('',#5115,#5112,#740,.T.);
#6558=EDGE_CURVE('',#5118,#5119,#741,.T.);
#6559=EDGE_CURVE('',#5119,#5118,#742,.T.);
#6560=EDGE_CURVE('',#5119,#5117,#3531,.T.);
#6561=EDGE_CURVE('',#5120,#5120,#1532,.T.);
#6562=EDGE_CURVE('',#5120,#5108,#3532,.T.);
#6563=EDGE_CURVE('',#5121,#5122,#743,.T.);
#6564=EDGE_CURVE('',#5121,#5123,#744,.T.);
#6565=EDGE_CURVE('',#5124,#5123,#745,.T.);
#6566=EDGE_CURVE('',#5122,#5124,#746,.T.);
#6567=EDGE_CURVE('',#5125,#5126,#747,.T.);
#6568=EDGE_CURVE('',#5127,#5125,#748,.T.);
#6569=EDGE_CURVE('',#5128,#5127,#749,.T.);
#6570=EDGE_CURVE('',#5126,#5128,#750,.T.);
#6571=EDGE_CURVE('',#5126,#5121,#751,.T.);
#6572=EDGE_CURVE('',#5123,#5128,#752,.T.);
#6573=EDGE_CURVE('',#5129,#5129,#1533,.T.);
#6574=EDGE_CURVE('',#5129,#5130,#3533,.T.);
#6575=EDGE_CURVE('',#5130,#5131,#753,.T.);
#6576=EDGE_CURVE('',#5131,#5132,#1534,.T.);
#6577=EDGE_CURVE('',#5132,#5133,#754,.T.);
#6578=EDGE_CURVE('',#5133,#5134,#755,.T.);
#6579=EDGE_CURVE('',#5134,#5135,#756,.T.);
#6580=EDGE_CURVE('',#5135,#5136,#1535,.T.);
#6581=EDGE_CURVE('',#5136,#5137,#757,.T.);
#6582=EDGE_CURVE('',#5137,#5138,#758,.T.);
#6583=EDGE_CURVE('',#5138,#5139,#759,.T.);
#6584=EDGE_CURVE('',#5139,#5140,#1536,.T.);
#6585=EDGE_CURVE('',#5140,#5141,#760,.T.);
#6586=EDGE_CURVE('',#5141,#5142,#761,.T.);
#6587=EDGE_CURVE('',#5142,#5143,#762,.T.);
#6588=EDGE_CURVE('',#5143,#5144,#1537,.T.);
#6589=EDGE_CURVE('',#5144,#5145,#763,.T.);
#6590=EDGE_CURVE('',#5145,#5146,#764,.T.);
#6591=EDGE_CURVE('',#5146,#5147,#765,.T.);
#6592=EDGE_CURVE('',#5147,#5148,#1538,.T.);
#6593=EDGE_CURVE('',#5148,#5149,#766,.T.);
#6594=EDGE_CURVE('',#5149,#5150,#767,.T.);
#6595=EDGE_CURVE('',#5150,#5151,#768,.T.);
#6596=EDGE_CURVE('',#5151,#5152,#1539,.T.);
#6597=EDGE_CURVE('',#5152,#5153,#769,.T.);
#6598=EDGE_CURVE('',#5153,#5154,#770,.T.);
#6599=EDGE_CURVE('',#5154,#5155,#771,.T.);
#6600=EDGE_CURVE('',#5155,#5156,#1540,.T.);
#6601=EDGE_CURVE('',#5156,#5157,#772,.T.);
#6602=EDGE_CURVE('',#5157,#5158,#773,.T.);
#6603=EDGE_CURVE('',#5158,#5159,#774,.T.);
#6604=EDGE_CURVE('',#5159,#5160,#1541,.T.);
#6605=EDGE_CURVE('',#5160,#5161,#775,.T.);
#6606=EDGE_CURVE('',#5161,#5162,#776,.T.);
#6607=EDGE_CURVE('',#5162,#5163,#777,.T.);
#6608=EDGE_CURVE('',#5163,#5164,#1542,.T.);
#6609=EDGE_CURVE('',#5164,#5165,#778,.T.);
#6610=EDGE_CURVE('',#5165,#5166,#779,.T.);
#6611=EDGE_CURVE('',#5166,#5167,#780,.T.);
#6612=EDGE_CURVE('',#5167,#5124,#1543,.T.);
#6613=EDGE_CURVE('',#5127,#5168,#1544,.T.);
#6614=EDGE_CURVE('',#5168,#5169,#781,.T.);
#6615=EDGE_CURVE('',#5169,#5170,#782,.T.);
#6616=EDGE_CURVE('',#5170,#5171,#783,.T.);
#6617=EDGE_CURVE('',#5171,#5172,#1545,.T.);
#6618=EDGE_CURVE('',#5172,#5173,#784,.T.);
#6619=EDGE_CURVE('',#5173,#5174,#785,.T.);
#6620=EDGE_CURVE('',#5174,#5175,#786,.T.);
#6621=EDGE_CURVE('',#5175,#5176,#1546,.T.);
#6622=EDGE_CURVE('',#5176,#5177,#787,.T.);
#6623=EDGE_CURVE('',#5177,#5178,#788,.T.);
#6624=EDGE_CURVE('',#5178,#5179,#789,.T.);
#6625=EDGE_CURVE('',#5179,#5180,#1547,.T.);
#6626=EDGE_CURVE('',#5180,#5181,#790,.T.);
#6627=EDGE_CURVE('',#5181,#5182,#791,.T.);
#6628=EDGE_CURVE('',#5182,#5183,#792,.T.);
#6629=EDGE_CURVE('',#5183,#5184,#1548,.T.);
#6630=EDGE_CURVE('',#5184,#5185,#793,.T.);
#6631=EDGE_CURVE('',#5185,#5186,#794,.T.);
#6632=EDGE_CURVE('',#5186,#5187,#795,.T.);
#6633=EDGE_CURVE('',#5187,#5188,#1549,.T.);
#6634=EDGE_CURVE('',#5188,#5189,#796,.T.);
#6635=EDGE_CURVE('',#5189,#5190,#797,.T.);
#6636=EDGE_CURVE('',#5190,#5191,#798,.T.);
#6637=EDGE_CURVE('',#5191,#5192,#1550,.T.);
#6638=EDGE_CURVE('',#5192,#5193,#799,.T.);
#6639=EDGE_CURVE('',#5193,#5194,#800,.T.);
#6640=EDGE_CURVE('',#5194,#5195,#801,.T.);
#6641=EDGE_CURVE('',#5195,#5196,#1551,.T.);
#6642=EDGE_CURVE('',#5196,#5197,#802,.T.);
#6643=EDGE_CURVE('',#5197,#5198,#803,.T.);
#6644=EDGE_CURVE('',#5198,#5199,#804,.T.);
#6645=EDGE_CURVE('',#5199,#5200,#1552,.T.);
#6646=EDGE_CURVE('',#5200,#5201,#805,.T.);
#6647=EDGE_CURVE('',#5201,#5202,#806,.T.);
#6648=EDGE_CURVE('',#5202,#5203,#807,.T.);
#6649=EDGE_CURVE('',#5203,#5204,#1553,.T.);
#6650=EDGE_CURVE('',#5204,#5205,#808,.T.);
#6651=EDGE_CURVE('',#5205,#5206,#809,.T.);
#6652=EDGE_CURVE('',#5206,#5130,#810,.T.);
#6653=EDGE_CURVE('',#5125,#5207,#1554,.T.);
#6654=EDGE_CURVE('',#5207,#5168,#811,.T.);
#6655=EDGE_CURVE('',#5167,#5208,#812,.T.);
#6656=EDGE_CURVE('',#5208,#5122,#1555,.T.);
#6657=EDGE_CURVE('',#5209,#5210,#813,.T.);
#6658=EDGE_CURVE('',#5209,#5165,#814,.T.);
#6659=EDGE_CURVE('',#5210,#5164,#815,.T.);
#6660=EDGE_CURVE('',#5208,#5211,#816,.T.);
#6661=EDGE_CURVE('',#5211,#5166,#817,.T.);
#6662=EDGE_CURVE('',#5211,#5209,#818,.T.);
#6663=EDGE_CURVE('',#5163,#5212,#819,.T.);
#6664=EDGE_CURVE('',#5212,#5210,#1556,.T.);
#6665=EDGE_CURVE('',#5213,#5214,#820,.T.);
#6666=EDGE_CURVE('',#5213,#5161,#821,.T.);
#6667=EDGE_CURVE('',#5214,#5160,#822,.T.);
#6668=EDGE_CURVE('',#5212,#5215,#823,.T.);
#6669=EDGE_CURVE('',#5215,#5162,#824,.T.);
#6670=EDGE_CURVE('',#5215,#5213,#825,.T.);
#6671=EDGE_CURVE('',#5159,#5216,#826,.T.);
#6672=EDGE_CURVE('',#5216,#5214,#1557,.T.);
#6673=EDGE_CURVE('',#5217,#5218,#827,.T.);
#6674=EDGE_CURVE('',#5217,#5157,#828,.T.);
#6675=EDGE_CURVE('',#5218,#5156,#829,.T.);
#6676=EDGE_CURVE('',#5216,#5219,#830,.T.);
#6677=EDGE_CURVE('',#5219,#5158,#831,.T.);
#6678=EDGE_CURVE('',#5219,#5217,#832,.T.);
#6679=EDGE_CURVE('',#5155,#5220,#833,.T.);
#6680=EDGE_CURVE('',#5220,#5218,#1558,.T.);
#6681=EDGE_CURVE('',#5221,#5222,#834,.T.);
#6682=EDGE_CURVE('',#5221,#5153,#835,.T.);
#6683=EDGE_CURVE('',#5222,#5152,#836,.T.);
#6684=EDGE_CURVE('',#5220,#5223,#837,.T.);
#6685=EDGE_CURVE('',#5223,#5154,#838,.T.);
#6686=EDGE_CURVE('',#5223,#5221,#839,.T.);
#6687=EDGE_CURVE('',#5151,#5224,#840,.T.);
#6688=EDGE_CURVE('',#5224,#5222,#1559,.T.);
#6689=EDGE_CURVE('',#5225,#5226,#841,.T.);
#6690=EDGE_CURVE('',#5225,#5149,#842,.T.);
#6691=EDGE_CURVE('',#5226,#5148,#843,.T.);
#6692=EDGE_CURVE('',#5224,#5227,#844,.T.);
#6693=EDGE_CURVE('',#5227,#5150,#845,.T.);
#6694=EDGE_CURVE('',#5227,#5225,#846,.T.);
#6695=EDGE_CURVE('',#5147,#5228,#847,.T.);
#6696=EDGE_CURVE('',#5228,#5226,#1560,.T.);
#6697=EDGE_CURVE('',#5229,#5230,#848,.T.);
#6698=EDGE_CURVE('',#5229,#5145,#849,.T.);
#6699=EDGE_CURVE('',#5230,#5144,#850,.T.);
#6700=EDGE_CURVE('',#5228,#5231,#851,.T.);
#6701=EDGE_CURVE('',#5231,#5146,#852,.T.);
#6702=EDGE_CURVE('',#5231,#5229,#853,.T.);
#6703=EDGE_CURVE('',#5143,#5232,#854,.T.);
#6704=EDGE_CURVE('',#5232,#5230,#1561,.T.);
#6705=EDGE_CURVE('',#5233,#5234,#855,.T.);
#6706=EDGE_CURVE('',#5233,#5141,#856,.T.);
#6707=EDGE_CURVE('',#5234,#5140,#857,.T.);
#6708=EDGE_CURVE('',#5232,#5235,#858,.T.);
#6709=EDGE_CURVE('',#5235,#5142,#859,.T.);
#6710=EDGE_CURVE('',#5235,#5233,#860,.T.);
#6711=EDGE_CURVE('',#5139,#5236,#861,.T.);
#6712=EDGE_CURVE('',#5236,#5234,#1562,.T.);
#6713=EDGE_CURVE('',#5237,#5238,#862,.T.);
#6714=EDGE_CURVE('',#5237,#5137,#863,.T.);
#6715=EDGE_CURVE('',#5238,#5136,#864,.T.);
#6716=EDGE_CURVE('',#5236,#5239,#865,.T.);
#6717=EDGE_CURVE('',#5239,#5138,#866,.T.);
#6718=EDGE_CURVE('',#5239,#5237,#867,.T.);
#6719=EDGE_CURVE('',#5135,#5240,#868,.T.);
#6720=EDGE_CURVE('',#5240,#5238,#1563,.T.);
#6721=EDGE_CURVE('',#5241,#5242,#869,.T.);
#6722=EDGE_CURVE('',#5241,#5133,#870,.T.);
#6723=EDGE_CURVE('',#5242,#5132,#871,.T.);
#6724=EDGE_CURVE('',#5240,#5243,#872,.T.);
#6725=EDGE_CURVE('',#5244,#5134,#873,.T.);
#6726=EDGE_CURVE('',#5243,#5244,#874,.T.);
#6727=EDGE_CURVE('',#5244,#5241,#875,.T.);
#6728=EDGE_CURVE('',#5131,#5245,#876,.T.);
#6729=EDGE_CURVE('',#5245,#5242,#1564,.T.);
#6730=EDGE_CURVE('',#5246,#5247,#877,.T.);
#6731=EDGE_CURVE('',#5246,#5205,#878,.T.);
#6732=EDGE_CURVE('',#5247,#5204,#879,.T.);
#6733=EDGE_CURVE('',#5245,#5248,#880,.T.);
#6734=EDGE_CURVE('',#5248,#5206,#881,.T.);
#6735=EDGE_CURVE('',#5248,#5246,#882,.T.);
#6736=EDGE_CURVE('',#5203,#5249,#883,.T.);
#6737=EDGE_CURVE('',#5249,#5247,#1565,.T.);
#6738=EDGE_CURVE('',#5250,#5251,#884,.T.);
#6739=EDGE_CURVE('',#5250,#5201,#885,.T.);
#6740=EDGE_CURVE('',#5251,#5200,#886,.T.);
#6741=EDGE_CURVE('',#5249,#5252,#887,.T.);
#6742=EDGE_CURVE('',#5252,#5202,#888,.T.);
#6743=EDGE_CURVE('',#5252,#5250,#889,.T.);
#6744=EDGE_CURVE('',#5199,#5253,#890,.T.);
#6745=EDGE_CURVE('',#5253,#5251,#1566,.T.);
#6746=EDGE_CURVE('',#5254,#5255,#891,.T.);
#6747=EDGE_CURVE('',#5254,#5197,#892,.T.);
#6748=EDGE_CURVE('',#5255,#5196,#893,.T.);
#6749=EDGE_CURVE('',#5253,#5256,#894,.T.);
#6750=EDGE_CURVE('',#5256,#5198,#895,.T.);
#6751=EDGE_CURVE('',#5256,#5254,#896,.T.);
#6752=EDGE_CURVE('',#5195,#5257,#897,.T.);
#6753=EDGE_CURVE('',#5257,#5255,#1567,.T.);
#6754=EDGE_CURVE('',#5258,#5259,#898,.T.);
#6755=EDGE_CURVE('',#5258,#5193,#899,.T.);
#6756=EDGE_CURVE('',#5259,#5192,#900,.T.);
#6757=EDGE_CURVE('',#5257,#5260,#901,.T.);
#6758=EDGE_CURVE('',#5260,#5194,#902,.T.);
#6759=EDGE_CURVE('',#5260,#5258,#903,.T.);
#6760=EDGE_CURVE('',#5191,#5261,#904,.T.);
#6761=EDGE_CURVE('',#5261,#5259,#1568,.T.);
#6762=EDGE_CURVE('',#5262,#5263,#905,.T.);
#6763=EDGE_CURVE('',#5262,#5189,#906,.T.);
#6764=EDGE_CURVE('',#5263,#5188,#907,.T.);
#6765=EDGE_CURVE('',#5261,#5264,#908,.T.);
#6766=EDGE_CURVE('',#5264,#5190,#909,.T.);
#6767=EDGE_CURVE('',#5264,#5262,#910,.T.);
#6768=EDGE_CURVE('',#5187,#5265,#911,.T.);
#6769=EDGE_CURVE('',#5265,#5263,#1569,.T.);
#6770=EDGE_CURVE('',#5266,#5267,#912,.T.);
#6771=EDGE_CURVE('',#5266,#5185,#913,.T.);
#6772=EDGE_CURVE('',#5267,#5184,#914,.T.);
#6773=EDGE_CURVE('',#5265,#5268,#915,.T.);
#6774=EDGE_CURVE('',#5268,#5186,#916,.T.);
#6775=EDGE_CURVE('',#5268,#5266,#917,.T.);
#6776=EDGE_CURVE('',#5183,#5269,#918,.T.);
#6777=EDGE_CURVE('',#5269,#5267,#1570,.T.);
#6778=EDGE_CURVE('',#5270,#5271,#919,.T.);
#6779=EDGE_CURVE('',#5270,#5181,#920,.T.);
#6780=EDGE_CURVE('',#5271,#5180,#921,.T.);
#6781=EDGE_CURVE('',#5269,#5272,#922,.T.);
#6782=EDGE_CURVE('',#5272,#5182,#923,.T.);
#6783=EDGE_CURVE('',#5272,#5270,#924,.T.);
#6784=EDGE_CURVE('',#5179,#5273,#925,.T.);
#6785=EDGE_CURVE('',#5273,#5271,#1571,.T.);
#6786=EDGE_CURVE('',#5274,#5275,#926,.T.);
#6787=EDGE_CURVE('',#5274,#5177,#927,.T.);
#6788=EDGE_CURVE('',#5275,#5176,#928,.T.);
#6789=EDGE_CURVE('',#5273,#5276,#929,.T.);
#6790=EDGE_CURVE('',#5276,#5178,#930,.T.);
#6791=EDGE_CURVE('',#5276,#5274,#931,.T.);
#6792=EDGE_CURVE('',#5175,#5277,#932,.T.);
#6793=EDGE_CURVE('',#5277,#5275,#1572,.T.);
#6794=EDGE_CURVE('',#5278,#5174,#933,.T.);
#6795=EDGE_CURVE('',#5277,#5278,#934,.T.);
#6796=EDGE_CURVE('',#5279,#5173,#935,.T.);
#6797=EDGE_CURVE('',#5278,#5279,#936,.T.);
#6798=EDGE_CURVE('',#5280,#5172,#937,.T.);
#6799=EDGE_CURVE('',#5279,#5280,#938,.T.);
#6800=EDGE_CURVE('',#5281,#5170,#939,.T.);
#6801=EDGE_CURVE('',#5282,#5281,#940,.T.);
#6802=EDGE_CURVE('',#5171,#5282,#941,.T.);
#6803=EDGE_CURVE('',#5283,#5169,#942,.T.);
#6804=EDGE_CURVE('',#5281,#5283,#943,.T.);
#6805=EDGE_CURVE('',#5283,#5207,#944,.T.);
#6806=EDGE_CURVE('',#5284,#5284,#1573,.T.);
#6807=EDGE_CURVE('',#5284,#5243,#3534,.T.);
#6808=EDGE_CURVE('',#5282,#5280,#1574,.T.);
#6809=EDGE_CURVE('',#5285,#5285,#1575,.T.);
#6810=EDGE_CURVE('',#5285,#5286,#3535,.T.);
#6811=EDGE_CURVE('',#5286,#5286,#1576,.T.);
#6812=EDGE_CURVE('',#5286,#5287,#3536,.T.);
#6813=EDGE_CURVE('',#5287,#5287,#1577,.T.);
#6814=EDGE_CURVE('',#5287,#5288,#3537,.T.);
#6815=EDGE_CURVE('',#5288,#5288,#1578,.T.);
#6816=EDGE_CURVE('',#5289,#5289,#1579,.T.);
#6817=EDGE_CURVE('',#5290,#5290,#1580,.T.);
#6818=EDGE_CURVE('',#5291,#5291,#1581,.T.);
#6819=EDGE_CURVE('',#5292,#5292,#1582,.T.);
#6820=EDGE_CURVE('',#5292,#5290,#3538,.T.);
#6821=EDGE_CURVE('',#5293,#5293,#1583,.T.);
#6822=EDGE_CURVE('',#5293,#5291,#3539,.T.);
#6823=EDGE_CURVE('',#5294,#5294,#1584,.T.);
#6824=EDGE_CURVE('',#5295,#5295,#1585,.T.);
#6825=EDGE_CURVE('',#5296,#5296,#1586,.T.);
#6826=EDGE_CURVE('',#5297,#5297,#1587,.T.);
#6827=EDGE_CURVE('',#5297,#5295,#3540,.T.);
#6828=EDGE_CURVE('',#5298,#5299,#945,.T.);
#6829=EDGE_CURVE('',#5299,#5300,#1588,.T.);
#6830=EDGE_CURVE('',#5300,#5301,#946,.T.);
#6831=EDGE_CURVE('',#5301,#5302,#1589,.T.);
#6832=EDGE_CURVE('',#5302,#5303,#947,.T.);
#6833=EDGE_CURVE('',#5303,#5304,#1590,.T.);
#6834=EDGE_CURVE('',#5304,#5305,#948,.T.);
#6835=EDGE_CURVE('',#5305,#5306,#1591,.T.);
#6836=EDGE_CURVE('',#5306,#5307,#949,.T.);
#6837=EDGE_CURVE('',#5307,#5308,#1592,.T.);
#6838=EDGE_CURVE('',#5308,#5296,#3541,.T.);
#6839=EDGE_CURVE('',#5308,#5309,#1593,.T.);
#6840=EDGE_CURVE('',#5309,#5310,#950,.T.);
#6841=EDGE_CURVE('',#5310,#5311,#1594,.T.);
#6842=EDGE_CURVE('',#5311,#5312,#951,.T.);
#6843=EDGE_CURVE('',#5312,#5298,#1595,.T.);
#6844=EDGE_CURVE('',#5313,#5314,#952,.T.);
#6845=EDGE_CURVE('',#5315,#5313,#953,.T.);
#6846=EDGE_CURVE('',#5316,#5315,#954,.T.);
#6847=EDGE_CURVE('',#5316,#5317,#1596,.T.);
#6848=EDGE_CURVE('',#5318,#5316,#955,.T.);
#6849=EDGE_CURVE('',#5319,#5318,#956,.T.);
#6850=EDGE_CURVE('',#5314,#5319,#957,.T.);
#6851=EDGE_CURVE('',#5320,#5314,#1597,.T.);
#6852=EDGE_CURVE('',#5321,#5298,#958,.T.);
#6853=EDGE_CURVE('',#5322,#5321,#959,.T.);
#6854=EDGE_CURVE('',#5299,#5322,#960,.T.);
#6855=EDGE_CURVE('',#5289,#5323,#3542,.T.);
#6856=EDGE_CURVE('',#5323,#5324,#1598,.T.);
#6857=EDGE_CURVE('',#5324,#5325,#961,.T.);
#6858=EDGE_CURVE('',#5325,#5326,#1599,.T.);
#6859=EDGE_CURVE('',#5326,#5327,#962,.T.);
#6860=EDGE_CURVE('',#5327,#5328,#1600,.T.);
#6861=EDGE_CURVE('',#5328,#5329,#963,.T.);
#6862=EDGE_CURVE('',#5329,#5330,#1601,.T.);
#6863=EDGE_CURVE('',#5330,#5331,#964,.T.);
#6864=EDGE_CURVE('',#5331,#5322,#1602,.T.);
#6865=EDGE_CURVE('',#5321,#5332,#1603,.T.);
#6866=EDGE_CURVE('',#5332,#5333,#965,.T.);
#6867=EDGE_CURVE('',#5333,#5334,#1604,.T.);
#6868=EDGE_CURVE('',#5334,#5335,#966,.T.);
#6869=EDGE_CURVE('',#5335,#5323,#1605,.T.);
#6870=EDGE_CURVE('',#5312,#5332,#967,.T.);
#6871=EDGE_CURVE('',#5315,#5336,#1606,.T.);
#6872=EDGE_CURVE('',#5336,#5337,#968,.T.);
#6873=EDGE_CURVE('',#5337,#5338,#969,.T.);
#6874=EDGE_CURVE('',#5338,#5339,#1607,.T.);
#6875=EDGE_CURVE('',#5339,#5340,#970,.T.);
#6876=EDGE_CURVE('',#5340,#5341,#971,.T.);
#6877=EDGE_CURVE('',#5341,#5342,#1608,.T.);
#6878=EDGE_CURVE('',#5342,#5343,#3543,.T.);
#6879=EDGE_CURVE('',#5343,#5343,#1609,.T.);
#6880=EDGE_CURVE('',#5342,#5344,#1610,.T.);
#6881=EDGE_CURVE('',#5344,#5345,#972,.T.);
#6882=EDGE_CURVE('',#5345,#5346,#973,.T.);
#6883=EDGE_CURVE('',#5346,#5347,#1611,.T.);
#6884=EDGE_CURVE('',#5347,#5348,#974,.T.);
#6885=EDGE_CURVE('',#5348,#5349,#975,.T.);
#6886=EDGE_CURVE('',#5349,#5350,#1612,.T.);
#6887=EDGE_CURVE('',#5350,#5351,#976,.T.);
#6888=EDGE_CURVE('',#5351,#5352,#977,.T.);
#6889=EDGE_CURVE('',#5352,#5353,#1613,.T.);
#6890=EDGE_CURVE('',#5353,#5354,#978,.T.);
#6891=EDGE_CURVE('',#5354,#5355,#979,.T.);
#6892=EDGE_CURVE('',#5355,#5318,#1614,.T.);
#6893=EDGE_CURVE('',#5356,#5313,#1615,.T.);
#6894=EDGE_CURVE('',#5356,#5336,#980,.T.);
#6895=EDGE_CURVE('',#5357,#5358,#981,.T.);
#6896=EDGE_CURVE('',#5338,#5357,#982,.T.);
#6897=EDGE_CURVE('',#5337,#5359,#1616,.T.);
#6898=EDGE_CURVE('',#5358,#5356,#983,.T.);
#6899=EDGE_CURVE('',#5360,#5358,#1617,.T.);
#6900=EDGE_CURVE('',#5333,#5311,#984,.T.);
#6901=EDGE_CURVE('',#5310,#5334,#985,.T.);
#6902=EDGE_CURVE('',#5361,#5357,#1618,.T.);
#6903=EDGE_CURVE('',#5361,#5339,#986,.T.);
#6904=EDGE_CURVE('',#5362,#5363,#987,.T.);
#6905=EDGE_CURVE('',#5341,#5362,#988,.T.);
#6906=EDGE_CURVE('',#5340,#5364,#1619,.T.);
#6907=EDGE_CURVE('',#5363,#5361,#989,.T.);
#6908=EDGE_CURVE('',#5365,#5363,#1620,.T.);
#6909=EDGE_CURVE('',#5335,#5309,#990,.T.);
#6910=EDGE_CURVE('',#5307,#5324,#991,.T.);
#6911=EDGE_CURVE('',#5366,#5362,#1621,.T.);
#6912=EDGE_CURVE('',#5367,#5366,#1622,.T.);
#6913=EDGE_CURVE('',#5367,#5344,#992,.T.);
#6914=EDGE_CURVE('',#5368,#5369,#993,.T.);
#6915=EDGE_CURVE('',#5346,#5368,#994,.T.);
#6916=EDGE_CURVE('',#5345,#5370,#1623,.T.);
#6917=EDGE_CURVE('',#5369,#5367,#995,.T.);
#6918=EDGE_CURVE('',#5371,#5369,#1624,.T.);
#6919=EDGE_CURVE('',#5325,#5306,#996,.T.);
#6920=EDGE_CURVE('',#5305,#5326,#997,.T.);
#6921=EDGE_CURVE('',#5372,#5368,#1625,.T.);
#6922=EDGE_CURVE('',#5372,#5347,#998,.T.);
#6923=EDGE_CURVE('',#5373,#5374,#999,.T.);
#6924=EDGE_CURVE('',#5349,#5373,#1000,.T.);
#6925=EDGE_CURVE('',#5348,#5375,#1626,.T.);
#6926=EDGE_CURVE('',#5374,#5372,#1001,.T.);
#6927=EDGE_CURVE('',#5376,#5374,#1627,.T.);
#6928=EDGE_CURVE('',#5327,#5304,#1002,.T.);
#6929=EDGE_CURVE('',#5303,#5328,#1003,.T.);
#6930=EDGE_CURVE('',#5377,#5373,#1628,.T.);
#6931=EDGE_CURVE('',#5377,#5350,#1004,.T.);
#6932=EDGE_CURVE('',#5378,#5377,#1005,.T.);
#6933=EDGE_CURVE('',#5379,#5378,#1629,.T.);
#6934=EDGE_CURVE('',#5380,#5378,#1006,.T.);
#6935=EDGE_CURVE('',#5352,#5380,#1007,.T.);
#6936=EDGE_CURVE('',#5351,#5381,#1630,.T.);
#6937=EDGE_CURVE('',#5329,#5302,#1008,.T.);
#6938=EDGE_CURVE('',#5294,#5382,#3544,.T.);
#6939=EDGE_CURVE('',#5382,#5382,#1631,.T.);
#6940=EDGE_CURVE('',#5331,#5300,#1009,.T.);
#6941=EDGE_CURVE('',#5383,#5383,#1632,.T.);
#6942=EDGE_CURVE('',#5383,#5366,#3545,.T.);
#6943=EDGE_CURVE('',#5319,#5384,#1633,.T.);
#6944=EDGE_CURVE('',#5384,#5385,#1010,.T.);
#6945=EDGE_CURVE('',#5385,#5386,#1011,.T.);
#6946=EDGE_CURVE('',#5386,#5380,#1634,.T.);
#6947=EDGE_CURVE('',#5355,#5384,#1012,.T.);
#6948=EDGE_CURVE('',#5354,#5387,#1635,.T.);
#6949=EDGE_CURVE('',#5386,#5353,#1013,.T.);
#6950=EDGE_CURVE('',#5388,#5385,#1636,.T.);
#6951=EDGE_CURVE('',#5301,#5330,#1014,.T.);
#6952=EDGE_CURVE('',#5389,#5389,#1637,.T.);
#6953=EDGE_CURVE('',#5390,#5390,#1638,.T.);
#6954=EDGE_CURVE('',#5390,#5389,#3546,.T.);
#6955=EDGE_CURVE('',#5391,#5391,#1639,.T.);
#6956=EDGE_CURVE('',#5391,#5390,#3547,.T.);
#6957=EDGE_CURVE('',#5392,#5392,#1640,.T.);
#6958=EDGE_CURVE('',#5392,#5391,#3548,.T.);
#6959=EDGE_CURVE('',#5393,#5393,#1641,.T.);
#6960=EDGE_CURVE('',#5393,#5394,#3549,.T.);
#6961=EDGE_CURVE('',#5394,#5394,#1642,.T.);
#6962=EDGE_CURVE('',#5394,#5395,#3550,.T.);
#6963=EDGE_CURVE('',#5395,#5395,#1643,.T.);
#6964=EDGE_CURVE('',#5396,#5396,#1644,.T.);
#6965=EDGE_CURVE('',#5396,#5393,#3551,.T.);
#6966=EDGE_CURVE('',#5397,#5397,#1645,.T.);
#6967=EDGE_CURVE('',#5397,#5398,#3552,.T.);
#6968=EDGE_CURVE('',#5398,#5398,#1646,.T.);
#6969=EDGE_CURVE('',#5399,#5399,#1647,.T.);
#6970=EDGE_CURVE('',#5400,#5400,#1648,.T.);
#6971=EDGE_CURVE('',#5400,#5399,#3553,.T.);
#6972=EDGE_CURVE('',#5401,#5402,#3554,.T.);
#6973=EDGE_CURVE('',#5402,#5403,#3555,.T.);
#6974=EDGE_CURVE('',#5403,#5404,#172,.T.);
#6975=EDGE_CURVE('',#5404,#5401,#3556,.T.);
#6976=EDGE_CURVE('',#5402,#5405,#3557,.T.);
#6977=EDGE_CURVE('',#5406,#5405,#3558,.T.);
#6978=EDGE_CURVE('',#5403,#5406,#3559,.T.);
#6979=EDGE_CURVE('',#5401,#5407,#3560,.T.);
#6980=EDGE_CURVE('',#5407,#5408,#3561,.T.);
#6981=EDGE_CURVE('',#5409,#5408,#3562,.T.);
#6982=EDGE_CURVE('',#5405,#5409,#3563,.T.);
#6983=EDGE_CURVE('',#5410,#5411,#3564,.T.);
#6984=EDGE_CURVE('',#5411,#5412,#3565,.T.);
#6985=EDGE_CURVE('',#5412,#5413,#173,.T.);
#6986=EDGE_CURVE('',#5413,#5410,#3566,.T.);
#6987=EDGE_CURVE('',#5414,#5413,#3567,.T.);
#6988=EDGE_CURVE('',#5415,#5414,#3568,.T.);
#6989=EDGE_CURVE('',#5410,#5415,#3569,.T.);
#6990=EDGE_CURVE('',#5416,#5406,#174,.T.);
#6991=EDGE_CURVE('',#5417,#5416,#1649,.T.);
#6992=EDGE_CURVE('',#5414,#5417,#175,.T.);
#6993=EDGE_CURVE('',#5412,#5404,#1650,.T.);
#6994=EDGE_CURVE('',#5409,#5416,#3570,.T.);
#6995=EDGE_CURVE('',#5408,#5418,#3571,.T.);
#6996=EDGE_CURVE('',#5418,#5419,#3572,.T.);
#6997=EDGE_CURVE('',#5419,#5420,#1651,.T.);
#6998=EDGE_CURVE('',#5420,#5421,#3573,.T.);
#6999=EDGE_CURVE('',#5421,#5422,#3574,.T.);
#7000=EDGE_CURVE('',#5422,#5423,#3575,.T.);
#7001=EDGE_CURVE('',#5417,#5423,#3576,.T.);
#7002=EDGE_CURVE('',#5424,#5424,#1652,.T.);
#7003=EDGE_CURVE('',#5425,#5425,#1653,.T.);
#7004=EDGE_CURVE('',#5423,#5415,#3577,.T.);
#7005=EDGE_CURVE('',#5426,#5422,#3578,.T.);
#7006=EDGE_CURVE('',#5411,#5426,#3579,.T.);
#7007=EDGE_CURVE('',#5427,#5427,#1654,.T.);
#7008=EDGE_CURVE('',#5427,#5425,#3580,.T.);
#7009=EDGE_CURVE('',#5428,#5428,#1655,.T.);
#7010=EDGE_CURVE('',#5428,#5424,#3581,.T.);
#7011=EDGE_CURVE('',#5429,#5420,#3582,.T.);
#7012=EDGE_CURVE('',#5430,#5429,#3583,.T.);
#7013=EDGE_CURVE('',#5430,#5421,#3584,.T.);
#7014=EDGE_CURVE('',#5426,#5430,#3585,.T.);
#7015=EDGE_CURVE('',#5419,#5431,#3586,.T.);
#7016=EDGE_CURVE('',#5432,#5418,#3587,.T.);
#7017=EDGE_CURVE('',#5432,#5431,#3588,.T.);
#7018=EDGE_CURVE('',#5407,#5432,#3589,.T.);
#7019=EDGE_CURVE('',#5431,#5429,#1656,.T.);
#7020=EDGE_CURVE('',#5433,#5434,#3590,.T.);
#7021=EDGE_CURVE('',#5433,#5435,#1015,.T.);
#7022=EDGE_CURVE('',#5435,#5436,#1657,.T.);
#7023=EDGE_CURVE('',#5436,#5434,#1016,.T.);
#7024=EDGE_CURVE('',#5437,#5438,#3591,.T.);
#7025=EDGE_CURVE('',#5437,#5433,#1017,.T.);
#7026=EDGE_CURVE('',#5434,#5438,#1018,.T.);
#7027=EDGE_CURVE('',#5439,#5440,#3592,.T.);
#7028=EDGE_CURVE('',#5439,#5437,#1019,.T.);
#7029=EDGE_CURVE('',#5438,#5440,#1020,.T.);
#7030=EDGE_CURVE('',#5441,#5442,#3593,.T.);
#7031=EDGE_CURVE('',#5441,#5439,#1021,.T.);
#7032=EDGE_CURVE('',#5440,#5442,#1022,.T.);
#7033=EDGE_CURVE('',#5443,#5444,#3594,.T.);
#7034=EDGE_CURVE('',#5443,#5441,#1023,.T.);
#7035=EDGE_CURVE('',#5442,#5444,#1024,.T.);
#7036=EDGE_CURVE('',#5445,#5446,#3595,.T.);
#7037=EDGE_CURVE('',#5445,#5443,#1025,.T.);
#7038=EDGE_CURVE('',#5444,#5446,#1026,.T.);
#7039=EDGE_CURVE('',#5447,#5448,#3596,.T.);
#7040=EDGE_CURVE('',#5447,#5449,#1027,.T.);
#7041=EDGE_CURVE('',#5448,#5449,#1658,.T.);
#7042=EDGE_CURVE('',#5450,#5451,#3597,.T.);
#7043=EDGE_CURVE('',#5450,#5447,#1028,.T.);
#7044=EDGE_CURVE('',#5452,#5448,#1659,.T.);
#7045=EDGE_CURVE('',#5451,#5452,#1029,.T.);
#7046=EDGE_CURVE('',#5453,#5454,#3598,.T.);
#7047=EDGE_CURVE('',#5453,#5450,#1030,.T.);
#7048=EDGE_CURVE('',#5454,#5451,#1031,.T.);
#7049=EDGE_CURVE('',#5455,#5456,#3599,.T.);
#7050=EDGE_CURVE('',#5455,#5453,#1032,.T.);
#7051=EDGE_CURVE('',#5456,#5454,#1033,.T.);
#7052=EDGE_CURVE('',#5457,#5458,#3600,.T.);
#7053=EDGE_CURVE('',#5457,#5455,#1034,.T.);
#7054=EDGE_CURVE('',#5458,#5456,#1035,.T.);
#7055=EDGE_CURVE('',#5459,#5460,#3601,.T.);
#7056=EDGE_CURVE('',#5459,#5457,#1036,.T.);
#7057=EDGE_CURVE('',#5460,#5458,#1037,.T.);
#7058=EDGE_CURVE('',#5449,#5461,#1038,.T.);
#7059=EDGE_CURVE('',#5462,#5461,#1660,.F.);
#7060=EDGE_CURVE('',#5463,#5462,#1661,.F.);
#7061=EDGE_CURVE('',#5463,#5452,#1039,.T.);
#7062=EDGE_CURVE('',#5446,#5463,#1040,.T.);
#7063=EDGE_CURVE('',#5464,#5436,#1041,.T.);
#7064=EDGE_CURVE('',#5464,#5460,#1042,.T.);
#7065=EDGE_CURVE('',#5436,#5465,#1662,.T.);
#7066=EDGE_CURVE('',#5465,#5435,#1663,.T.);
#7067=EDGE_CURVE('',#5435,#5466,#1043,.T.);
#7068=EDGE_CURVE('',#5466,#5464,#1664,.T.);
#7069=EDGE_CURVE('',#5466,#5459,#1044,.T.);
#7070=EDGE_CURVE('',#5461,#5445,#1045,.T.);
#7071=EDGE_CURVE('',#5467,#5468,#3602,.T.);
#7072=EDGE_CURVE('',#5467,#5469,#3603,.T.);
#7073=EDGE_CURVE('',#5469,#5470,#3604,.T.);
#7074=EDGE_CURVE('',#5468,#5470,#3605,.T.);
#7075=EDGE_CURVE('',#5471,#5467,#3606,.T.);
#7076=EDGE_CURVE('',#5471,#5472,#3607,.T.);
#7077=EDGE_CURVE('',#5472,#5469,#3608,.T.);
#7078=EDGE_CURVE('',#5473,#5471,#3609,.T.);
#7079=EDGE_CURVE('',#5473,#5474,#3610,.T.);
#7080=EDGE_CURVE('',#5474,#5472,#3611,.T.);
#7081=EDGE_CURVE('',#5475,#5473,#3612,.T.);
#7082=EDGE_CURVE('',#5475,#5476,#3613,.T.);
#7083=EDGE_CURVE('',#5476,#5474,#3614,.T.);
#7084=EDGE_CURVE('',#5477,#5475,#3615,.T.);
#7085=EDGE_CURVE('',#5477,#5478,#3616,.T.);
#7086=EDGE_CURVE('',#5478,#5476,#3617,.T.);
#7087=EDGE_CURVE('',#5468,#5477,#3618,.T.);
#7088=EDGE_CURVE('',#5470,#5478,#3619,.T.);
#7089=EDGE_CURVE('',#5479,#5479,#1665,.T.);
#7090=EDGE_CURVE('',#5465,#5479,#3620,.T.);
#7091=EDGE_CURVE('',#5461,#5463,#1666,.F.);
#7092=EDGE_CURVE('',#5480,#5480,#1667,.T.);
#7093=EDGE_CURVE('',#5480,#5462,#3621,.T.);
#7094=EDGE_CURVE('',#5481,#5482,#3622,.T.);
#7095=EDGE_CURVE('',#5481,#5483,#1046,.T.);
#7096=EDGE_CURVE('',#5483,#5484,#1668,.T.);
#7097=EDGE_CURVE('',#5484,#5482,#1047,.T.);
#7098=EDGE_CURVE('',#5485,#5486,#3623,.T.);
#7099=EDGE_CURVE('',#5485,#5481,#1048,.T.);
#7100=EDGE_CURVE('',#5482,#5486,#1049,.T.);
#7101=EDGE_CURVE('',#5487,#5488,#3624,.T.);
#7102=EDGE_CURVE('',#5487,#5485,#1050,.T.);
#7103=EDGE_CURVE('',#5486,#5488,#1051,.T.);
#7104=EDGE_CURVE('',#5489,#5490,#3625,.T.);
#7105=EDGE_CURVE('',#5489,#5487,#1052,.T.);
#7106=EDGE_CURVE('',#5488,#5490,#1053,.T.);
#7107=EDGE_CURVE('',#5491,#5492,#3626,.T.);
#7108=EDGE_CURVE('',#5491,#5489,#1054,.T.);
#7109=EDGE_CURVE('',#5490,#5492,#1055,.T.);
#7110=EDGE_CURVE('',#5493,#5494,#3627,.T.);
#7111=EDGE_CURVE('',#5493,#5491,#1056,.T.);
#7112=EDGE_CURVE('',#5492,#5494,#1057,.T.);
#7113=EDGE_CURVE('',#5495,#5496,#3628,.T.);
#7114=EDGE_CURVE('',#5495,#5493,#1058,.T.);
#7115=EDGE_CURVE('',#5494,#5496,#1059,.T.);
#7116=EDGE_CURVE('',#5497,#5498,#3629,.T.);
#7117=EDGE_CURVE('',#5497,#5495,#1060,.T.);
#7118=EDGE_CURVE('',#5496,#5498,#1061,.T.);
#7119=EDGE_CURVE('',#5499,#5500,#3630,.T.);
#7120=EDGE_CURVE('',#5499,#5497,#1062,.T.);
#7121=EDGE_CURVE('',#5498,#5500,#1063,.T.);
#7122=EDGE_CURVE('',#5501,#5502,#3631,.T.);
#7123=EDGE_CURVE('',#5501,#5499,#1064,.T.);
#7124=EDGE_CURVE('',#5500,#5502,#1065,.T.);
#7125=EDGE_CURVE('',#5503,#5504,#3632,.T.);
#7126=EDGE_CURVE('',#5503,#5501,#1066,.T.);
#7127=EDGE_CURVE('',#5502,#5504,#1067,.T.);
#7128=EDGE_CURVE('',#5505,#5506,#3633,.T.);
#7129=EDGE_CURVE('',#5505,#5503,#1068,.T.);
#7130=EDGE_CURVE('',#5504,#5506,#1069,.T.);
#7131=EDGE_CURVE('',#5507,#5508,#3634,.T.);
#7132=EDGE_CURVE('',#5507,#5505,#1070,.T.);
#7133=EDGE_CURVE('',#5506,#5508,#1071,.T.);
#7134=EDGE_CURVE('',#5509,#5510,#3635,.T.);
#7135=EDGE_CURVE('',#5509,#5507,#1072,.T.);
#7136=EDGE_CURVE('',#5508,#5510,#1073,.T.);
#7137=EDGE_CURVE('',#5511,#5512,#3636,.T.);
#7138=EDGE_CURVE('',#5511,#5509,#1074,.T.);
#7139=EDGE_CURVE('',#5510,#5512,#1075,.T.);
#7140=EDGE_CURVE('',#5513,#5514,#3637,.T.);
#7141=EDGE_CURVE('',#5513,#5511,#1076,.T.);
#7142=EDGE_CURVE('',#5512,#5514,#1077,.T.);
#7143=EDGE_CURVE('',#5515,#5516,#3638,.T.);
#7144=EDGE_CURVE('',#5515,#5513,#1078,.T.);
#7145=EDGE_CURVE('',#5514,#5516,#1079,.T.);
#7146=EDGE_CURVE('',#5517,#5518,#3639,.T.);
#7147=EDGE_CURVE('',#5517,#5515,#1080,.T.);
#7148=EDGE_CURVE('',#5516,#5518,#1081,.T.);
#7149=EDGE_CURVE('',#5519,#5520,#3640,.T.);
#7150=EDGE_CURVE('',#5519,#5517,#1082,.T.);
#7151=EDGE_CURVE('',#5518,#5520,#1083,.T.);
#7152=EDGE_CURVE('',#5521,#5522,#3641,.T.);
#7153=EDGE_CURVE('',#5521,#5519,#1084,.T.);
#7154=EDGE_CURVE('',#5520,#5522,#1085,.T.);
#7155=EDGE_CURVE('',#5523,#5524,#3642,.T.);
#7156=EDGE_CURVE('',#5523,#5521,#1086,.T.);
#7157=EDGE_CURVE('',#5522,#5524,#1087,.T.);
#7158=EDGE_CURVE('',#5525,#5526,#3643,.T.);
#7159=EDGE_CURVE('',#5525,#5523,#1088,.T.);
#7160=EDGE_CURVE('',#5524,#5526,#1089,.T.);
#7161=EDGE_CURVE('',#5527,#5528,#3644,.T.);
#7162=EDGE_CURVE('',#5527,#5525,#1090,.T.);
#7163=EDGE_CURVE('',#5526,#5528,#1091,.T.);
#7164=EDGE_CURVE('',#5529,#5530,#3645,.T.);
#7165=EDGE_CURVE('',#5529,#5527,#1092,.T.);
#7166=EDGE_CURVE('',#5528,#5530,#1093,.T.);
#7167=EDGE_CURVE('',#5531,#5532,#3646,.T.);
#7168=EDGE_CURVE('',#5531,#5533,#1094,.T.);
#7169=EDGE_CURVE('',#5532,#5533,#1669,.T.);
#7170=EDGE_CURVE('',#5534,#5535,#3647,.T.);
#7171=EDGE_CURVE('',#5534,#5531,#1095,.T.);
#7172=EDGE_CURVE('',#5536,#5532,#1670,.T.);
#7173=EDGE_CURVE('',#5535,#5536,#1096,.T.);
#7174=EDGE_CURVE('',#5537,#5538,#3648,.T.);
#7175=EDGE_CURVE('',#5537,#5534,#1097,.T.);
#7176=EDGE_CURVE('',#5538,#5535,#1098,.T.);
#7177=EDGE_CURVE('',#5539,#5540,#3649,.T.);
#7178=EDGE_CURVE('',#5539,#5537,#1099,.T.);
#7179=EDGE_CURVE('',#5540,#5538,#1100,.T.);
#7180=EDGE_CURVE('',#5541,#5542,#3650,.T.);
#7181=EDGE_CURVE('',#5541,#5539,#1101,.T.);
#7182=EDGE_CURVE('',#5542,#5540,#1102,.T.);
#7183=EDGE_CURVE('',#5543,#5544,#3651,.T.);
#7184=EDGE_CURVE('',#5543,#5541,#1103,.T.);
#7185=EDGE_CURVE('',#5544,#5542,#1104,.T.);
#7186=EDGE_CURVE('',#5545,#5546,#3652,.T.);
#7187=EDGE_CURVE('',#5545,#5543,#1105,.T.);
#7188=EDGE_CURVE('',#5546,#5544,#1106,.T.);
#7189=EDGE_CURVE('',#5547,#5548,#3653,.T.);
#7190=EDGE_CURVE('',#5547,#5545,#1107,.T.);
#7191=EDGE_CURVE('',#5548,#5546,#1108,.T.);
#7192=EDGE_CURVE('',#5549,#5550,#3654,.T.);
#7193=EDGE_CURVE('',#5549,#5547,#1109,.T.);
#7194=EDGE_CURVE('',#5550,#5548,#1110,.T.);
#7195=EDGE_CURVE('',#5551,#5552,#3655,.T.);
#7196=EDGE_CURVE('',#5551,#5549,#1111,.T.);
#7197=EDGE_CURVE('',#5552,#5550,#1112,.T.);
#7198=EDGE_CURVE('',#5553,#5554,#3656,.T.);
#7199=EDGE_CURVE('',#5553,#5551,#1113,.T.);
#7200=EDGE_CURVE('',#5554,#5552,#1114,.T.);
#7201=EDGE_CURVE('',#5555,#5556,#3657,.T.);
#7202=EDGE_CURVE('',#5555,#5553,#1115,.T.);
#7203=EDGE_CURVE('',#5556,#5554,#1116,.T.);
#7204=EDGE_CURVE('',#5557,#5558,#3658,.T.);
#7205=EDGE_CURVE('',#5557,#5555,#1117,.T.);
#7206=EDGE_CURVE('',#5558,#5556,#1118,.T.);
#7207=EDGE_CURVE('',#5559,#5560,#3659,.T.);
#7208=EDGE_CURVE('',#5559,#5557,#1119,.T.);
#7209=EDGE_CURVE('',#5560,#5558,#1120,.T.);
#7210=EDGE_CURVE('',#5561,#5562,#3660,.T.);
#7211=EDGE_CURVE('',#5561,#5559,#1121,.T.);
#7212=EDGE_CURVE('',#5562,#5560,#1122,.T.);
#7213=EDGE_CURVE('',#5563,#5564,#3661,.T.);
#7214=EDGE_CURVE('',#5563,#5561,#1123,.T.);
#7215=EDGE_CURVE('',#5564,#5562,#1124,.T.);
#7216=EDGE_CURVE('',#5565,#5566,#3662,.T.);
#7217=EDGE_CURVE('',#5565,#5563,#1125,.T.);
#7218=EDGE_CURVE('',#5566,#5564,#1126,.T.);
#7219=EDGE_CURVE('',#5567,#5568,#3663,.T.);
#7220=EDGE_CURVE('',#5567,#5565,#1127,.T.);
#7221=EDGE_CURVE('',#5568,#5566,#1128,.T.);
#7222=EDGE_CURVE('',#5569,#5570,#3664,.T.);
#7223=EDGE_CURVE('',#5569,#5567,#1129,.T.);
#7224=EDGE_CURVE('',#5570,#5568,#1130,.T.);
#7225=EDGE_CURVE('',#5571,#5572,#3665,.T.);
#7226=EDGE_CURVE('',#5571,#5569,#1131,.T.);
#7227=EDGE_CURVE('',#5572,#5570,#1132,.T.);
#7228=EDGE_CURVE('',#5573,#5574,#3666,.T.);
#7229=EDGE_CURVE('',#5573,#5571,#1133,.T.);
#7230=EDGE_CURVE('',#5574,#5572,#1134,.T.);
#7231=EDGE_CURVE('',#5575,#5576,#3667,.T.);
#7232=EDGE_CURVE('',#5575,#5573,#1135,.T.);
#7233=EDGE_CURVE('',#5576,#5574,#1136,.T.);
#7234=EDGE_CURVE('',#5577,#5578,#3668,.T.);
#7235=EDGE_CURVE('',#5577,#5575,#1137,.T.);
#7236=EDGE_CURVE('',#5578,#5576,#1138,.T.);
#7237=EDGE_CURVE('',#5579,#5580,#3669,.T.);
#7238=EDGE_CURVE('',#5579,#5577,#1139,.T.);
#7239=EDGE_CURVE('',#5580,#5578,#1140,.T.);
#7240=EDGE_CURVE('',#5581,#5536,#1141,.T.);
#7241=EDGE_CURVE('',#5530,#5581,#1142,.T.);
#7242=EDGE_CURVE('',#5582,#5484,#1143,.T.);
#7243=EDGE_CURVE('',#5582,#5580,#1144,.T.);
#7244=EDGE_CURVE('',#5484,#5583,#1671,.T.);
#7245=EDGE_CURVE('',#5583,#5483,#1672,.T.);
#7246=EDGE_CURVE('',#5483,#5584,#1145,.T.);
#7247=EDGE_CURVE('',#5584,#5582,#1673,.T.);
#7248=EDGE_CURVE('',#5584,#5579,#1146,.T.);
#7249=EDGE_CURVE('',#5533,#5585,#1147,.T.);
#7250=EDGE_CURVE('',#5585,#5529,#1148,.T.);
#7251=EDGE_CURVE('',#5586,#5587,#3670,.T.);
#7252=EDGE_CURVE('',#5587,#5587,#1674,.T.);
#7253=EDGE_CURVE('',#5588,#5589,#3671,.T.);
#7254=EDGE_CURVE('',#5588,#5590,#3672,.T.);
#7255=EDGE_CURVE('',#5590,#5591,#3673,.T.);
#7256=EDGE_CURVE('',#5589,#5591,#3674,.T.);
#7257=EDGE_CURVE('',#5592,#5588,#3675,.T.);
#7258=EDGE_CURVE('',#5592,#5593,#3676,.T.);
#7259=EDGE_CURVE('',#5593,#5590,#3677,.T.);
#7260=EDGE_CURVE('',#5594,#5592,#3678,.T.);
#7261=EDGE_CURVE('',#5594,#5595,#3679,.T.);
#7262=EDGE_CURVE('',#5595,#5593,#3680,.T.);
#7263=EDGE_CURVE('',#5596,#5594,#3681,.T.);
#7264=EDGE_CURVE('',#5596,#5597,#3682,.T.);
#7265=EDGE_CURVE('',#5597,#5595,#3683,.T.);
#7266=EDGE_CURVE('',#5598,#5596,#3684,.T.);
#7267=EDGE_CURVE('',#5598,#5599,#3685,.T.);
#7268=EDGE_CURVE('',#5599,#5597,#3686,.T.);
#7269=EDGE_CURVE('',#5589,#5598,#3687,.T.);
#7270=EDGE_CURVE('',#5591,#5599,#3688,.T.);
#7271=EDGE_CURVE('',#5600,#5601,#3689,.T.);
#7272=EDGE_CURVE('',#5600,#5602,#3690,.T.);
#7273=EDGE_CURVE('',#5603,#5602,#3691,.T.);
#7274=EDGE_CURVE('',#5601,#5603,#3692,.T.);
#7275=EDGE_CURVE('',#5601,#5604,#1675,.T.);
#7276=EDGE_CURVE('',#5603,#5604,#3693,.T.);
#7277=EDGE_CURVE('',#5604,#5605,#3694,.T.);
#7278=EDGE_CURVE('',#5602,#5605,#3695,.T.);
#7279=EDGE_CURVE('',#5605,#5600,#1676,.T.);
#7280=EDGE_CURVE('',#5606,#5607,#3696,.T.);
#7281=EDGE_CURVE('',#5606,#5608,#3697,.T.);
#7282=EDGE_CURVE('',#5609,#5608,#3698,.T.);
#7283=EDGE_CURVE('',#5607,#5609,#3699,.T.);
#7284=EDGE_CURVE('',#5607,#5610,#1677,.T.);
#7285=EDGE_CURVE('',#5609,#5610,#3700,.T.);
#7286=EDGE_CURVE('',#5610,#5611,#3701,.T.);
#7287=EDGE_CURVE('',#5608,#5611,#3702,.T.);
#7288=EDGE_CURVE('',#5611,#5606,#1678,.T.);
#7289=EDGE_CURVE('',#5612,#5613,#3703,.T.);
#7290=EDGE_CURVE('',#5612,#5614,#3704,.T.);
#7291=EDGE_CURVE('',#5615,#5614,#3705,.T.);
#7292=EDGE_CURVE('',#5613,#5615,#3706,.T.);
#7293=EDGE_CURVE('',#5613,#5616,#1679,.T.);
#7294=EDGE_CURVE('',#5615,#5616,#3707,.T.);
#7295=EDGE_CURVE('',#5616,#5617,#3708,.T.);
#7296=EDGE_CURVE('',#5614,#5617,#3709,.T.);
#7297=EDGE_CURVE('',#5617,#5612,#1680,.T.);
#7298=EDGE_CURVE('',#5618,#5619,#3710,.T.);
#7299=EDGE_CURVE('',#5618,#5620,#3711,.T.);
#7300=EDGE_CURVE('',#5621,#5620,#3712,.T.);
#7301=EDGE_CURVE('',#5619,#5621,#3713,.T.);
#7302=EDGE_CURVE('',#5619,#5622,#1681,.T.);
#7303=EDGE_CURVE('',#5621,#5622,#3714,.T.);
#7304=EDGE_CURVE('',#5622,#5623,#3715,.T.);
#7305=EDGE_CURVE('',#5620,#5623,#3716,.T.);
#7306=EDGE_CURVE('',#5623,#5618,#1682,.T.);
#7307=EDGE_CURVE('',#5624,#5625,#3717,.T.);
#7308=EDGE_CURVE('',#5624,#5626,#3718,.T.);
#7309=EDGE_CURVE('',#5627,#5626,#3719,.T.);
#7310=EDGE_CURVE('',#5625,#5627,#3720,.T.);
#7311=EDGE_CURVE('',#5625,#5628,#1683,.T.);
#7312=EDGE_CURVE('',#5627,#5628,#3721,.T.);
#7313=EDGE_CURVE('',#5628,#5629,#3722,.T.);
#7314=EDGE_CURVE('',#5626,#5629,#3723,.T.);
#7315=EDGE_CURVE('',#5629,#5624,#1684,.T.);
#7316=EDGE_CURVE('',#5630,#5631,#3724,.T.);
#7317=EDGE_CURVE('',#5630,#5632,#3725,.T.);
#7318=EDGE_CURVE('',#5633,#5632,#3726,.T.);
#7319=EDGE_CURVE('',#5631,#5633,#3727,.T.);
#7320=EDGE_CURVE('',#5631,#5634,#1685,.T.);
#7321=EDGE_CURVE('',#5633,#5634,#3728,.T.);
#7322=EDGE_CURVE('',#5634,#5635,#3729,.T.);
#7323=EDGE_CURVE('',#5632,#5635,#3730,.T.);
#7324=EDGE_CURVE('',#5635,#5630,#1686,.T.);
#7325=EDGE_CURVE('',#5636,#5637,#3731,.T.);
#7326=EDGE_CURVE('',#5636,#5638,#3732,.T.);
#7327=EDGE_CURVE('',#5639,#5638,#3733,.T.);
#7328=EDGE_CURVE('',#5637,#5639,#3734,.T.);
#7329=EDGE_CURVE('',#5637,#5640,#1687,.T.);
#7330=EDGE_CURVE('',#5639,#5640,#3735,.T.);
#7331=EDGE_CURVE('',#5640,#5641,#3736,.T.);
#7332=EDGE_CURVE('',#5638,#5641,#3737,.T.);
#7333=EDGE_CURVE('',#5641,#5636,#1688,.T.);
#7334=EDGE_CURVE('',#5642,#5643,#3738,.T.);
#7335=EDGE_CURVE('',#5642,#5644,#3739,.T.);
#7336=EDGE_CURVE('',#5645,#5644,#3740,.T.);
#7337=EDGE_CURVE('',#5643,#5645,#3741,.T.);
#7338=EDGE_CURVE('',#5643,#5646,#1689,.T.);
#7339=EDGE_CURVE('',#5645,#5646,#3742,.T.);
#7340=EDGE_CURVE('',#5646,#5647,#3743,.T.);
#7341=EDGE_CURVE('',#5644,#5647,#3744,.T.);
#7342=EDGE_CURVE('',#5647,#5642,#1690,.T.);
#7343=EDGE_CURVE('',#5648,#5649,#3745,.T.);
#7344=EDGE_CURVE('',#5648,#5650,#3746,.T.);
#7345=EDGE_CURVE('',#5651,#5650,#3747,.T.);
#7346=EDGE_CURVE('',#5649,#5651,#3748,.T.);
#7347=EDGE_CURVE('',#5649,#5652,#1691,.T.);
#7348=EDGE_CURVE('',#5651,#5653,#3749,.T.);
#7349=EDGE_CURVE('',#5652,#5653,#1692,.T.);
#7350=EDGE_CURVE('',#5653,#5654,#3750,.T.);
#7351=EDGE_CURVE('',#5650,#5654,#3751,.T.);
#7352=EDGE_CURVE('',#5654,#5655,#1693,.T.);
#7353=EDGE_CURVE('',#5655,#5648,#1694,.T.);
#7354=EDGE_CURVE('',#5656,#5657,#3752,.T.);
#7355=EDGE_CURVE('',#5656,#5658,#3753,.T.);
#7356=EDGE_CURVE('',#5659,#5658,#3754,.T.);
#7357=EDGE_CURVE('',#5657,#5659,#3755,.T.);
#7358=EDGE_CURVE('',#5657,#5660,#1695,.T.);
#7359=EDGE_CURVE('',#5659,#5660,#3756,.T.);
#7360=EDGE_CURVE('',#5660,#5661,#3757,.T.);
#7361=EDGE_CURVE('',#5658,#5661,#3758,.T.);
#7362=EDGE_CURVE('',#5661,#5656,#1696,.T.);
#7363=EDGE_CURVE('',#5662,#5663,#3759,.T.);
#7364=EDGE_CURVE('',#5662,#5664,#3760,.T.);
#7365=EDGE_CURVE('',#5665,#5664,#3761,.T.);
#7366=EDGE_CURVE('',#5663,#5665,#3762,.T.);
#7367=EDGE_CURVE('',#5663,#5666,#1697,.T.);
#7368=EDGE_CURVE('',#5665,#5666,#3763,.T.);
#7369=EDGE_CURVE('',#5666,#5667,#3764,.T.);
#7370=EDGE_CURVE('',#5664,#5667,#3765,.T.);
#7371=EDGE_CURVE('',#5667,#5662,#1698,.T.);
#7372=EDGE_CURVE('',#5668,#5669,#3766,.T.);
#7373=EDGE_CURVE('',#5668,#5670,#3767,.T.);
#7374=EDGE_CURVE('',#5671,#5670,#3768,.T.);
#7375=EDGE_CURVE('',#5669,#5671,#3769,.T.);
#7376=EDGE_CURVE('',#5669,#5672,#1699,.T.);
#7377=EDGE_CURVE('',#5671,#5672,#3770,.T.);
#7378=EDGE_CURVE('',#5672,#5673,#3771,.T.);
#7379=EDGE_CURVE('',#5670,#5673,#3772,.T.);
#7380=EDGE_CURVE('',#5673,#5668,#1700,.T.);
#7381=EDGE_CURVE('',#5674,#5675,#3773,.T.);
#7382=EDGE_CURVE('',#5674,#5676,#3774,.T.);
#7383=EDGE_CURVE('',#5677,#5676,#3775,.T.);
#7384=EDGE_CURVE('',#5675,#5677,#3776,.T.);
#7385=EDGE_CURVE('',#5675,#5678,#1701,.T.);
#7386=EDGE_CURVE('',#5677,#5678,#3777,.T.);
#7387=EDGE_CURVE('',#5678,#5679,#3778,.T.);
#7388=EDGE_CURVE('',#5676,#5679,#3779,.T.);
#7389=EDGE_CURVE('',#5679,#5674,#1702,.T.);
#7390=EDGE_CURVE('',#5680,#5681,#3780,.T.);
#7391=EDGE_CURVE('',#5680,#5682,#3781,.T.);
#7392=EDGE_CURVE('',#5683,#5682,#3782,.T.);
#7393=EDGE_CURVE('',#5681,#5683,#3783,.T.);
#7394=EDGE_CURVE('',#5681,#5684,#1703,.T.);
#7395=EDGE_CURVE('',#5683,#5684,#3784,.T.);
#7396=EDGE_CURVE('',#5684,#5685,#3785,.T.);
#7397=EDGE_CURVE('',#5682,#5685,#3786,.T.);
#7398=EDGE_CURVE('',#5685,#5680,#1704,.T.);
#7399=EDGE_CURVE('',#5686,#5687,#3787,.T.);
#7400=EDGE_CURVE('',#5686,#5688,#3788,.T.);
#7401=EDGE_CURVE('',#5689,#5688,#3789,.T.);
#7402=EDGE_CURVE('',#5687,#5689,#3790,.T.);
#7403=EDGE_CURVE('',#5687,#5690,#1705,.T.);
#7404=EDGE_CURVE('',#5689,#5690,#3791,.T.);
#7405=EDGE_CURVE('',#5690,#5691,#3792,.T.);
#7406=EDGE_CURVE('',#5688,#5691,#3793,.T.);
#7407=EDGE_CURVE('',#5691,#5686,#1706,.T.);
#7408=EDGE_CURVE('',#5692,#5693,#3794,.T.);
#7409=EDGE_CURVE('',#5692,#5694,#3795,.T.);
#7410=EDGE_CURVE('',#5695,#5694,#3796,.T.);
#7411=EDGE_CURVE('',#5693,#5695,#3797,.T.);
#7412=EDGE_CURVE('',#5693,#5696,#1707,.T.);
#7413=EDGE_CURVE('',#5695,#5696,#3798,.T.);
#7414=EDGE_CURVE('',#5696,#5697,#3799,.T.);
#7415=EDGE_CURVE('',#5694,#5697,#3800,.T.);
#7416=EDGE_CURVE('',#5697,#5692,#1708,.T.);
#7417=EDGE_CURVE('',#5698,#5699,#3801,.T.);
#7418=EDGE_CURVE('',#5698,#5700,#3802,.T.);
#7419=EDGE_CURVE('',#5701,#5700,#3803,.T.);
#7420=EDGE_CURVE('',#5699,#5701,#3804,.T.);
#7421=EDGE_CURVE('',#5699,#5702,#1709,.T.);
#7422=EDGE_CURVE('',#5701,#5702,#3805,.T.);
#7423=EDGE_CURVE('',#5702,#5703,#3806,.T.);
#7424=EDGE_CURVE('',#5700,#5703,#3807,.T.);
#7425=EDGE_CURVE('',#5703,#5698,#1710,.T.);
#7426=EDGE_CURVE('',#5704,#5705,#3808,.T.);
#7427=EDGE_CURVE('',#5704,#5706,#3809,.T.);
#7428=EDGE_CURVE('',#5707,#5706,#3810,.T.);
#7429=EDGE_CURVE('',#5705,#5707,#3811,.T.);
#7430=EDGE_CURVE('',#5705,#5708,#1711,.T.);
#7431=EDGE_CURVE('',#5707,#5708,#3812,.T.);
#7432=EDGE_CURVE('',#5708,#5709,#3813,.T.);
#7433=EDGE_CURVE('',#5706,#5709,#3814,.T.);
#7434=EDGE_CURVE('',#5709,#5704,#1712,.T.);
#7435=EDGE_CURVE('',#5710,#5711,#3815,.T.);
#7436=EDGE_CURVE('',#5710,#5712,#3816,.T.);
#7437=EDGE_CURVE('',#5713,#5712,#3817,.T.);
#7438=EDGE_CURVE('',#5711,#5713,#3818,.T.);
#7439=EDGE_CURVE('',#5711,#5714,#1713,.T.);
#7440=EDGE_CURVE('',#5713,#5714,#3819,.T.);
#7441=EDGE_CURVE('',#5714,#5715,#3820,.T.);
#7442=EDGE_CURVE('',#5712,#5715,#3821,.T.);
#7443=EDGE_CURVE('',#5715,#5710,#1714,.T.);
#7444=EDGE_CURVE('',#5716,#5717,#3822,.T.);
#7445=EDGE_CURVE('',#5716,#5718,#3823,.T.);
#7446=EDGE_CURVE('',#5719,#5718,#3824,.T.);
#7447=EDGE_CURVE('',#5717,#5719,#3825,.T.);
#7448=EDGE_CURVE('',#5717,#5720,#1715,.T.);
#7449=EDGE_CURVE('',#5719,#5720,#3826,.T.);
#7450=EDGE_CURVE('',#5720,#5721,#3827,.T.);
#7451=EDGE_CURVE('',#5718,#5721,#3828,.T.);
#7452=EDGE_CURVE('',#5721,#5716,#1716,.T.);
#7453=EDGE_CURVE('',#5722,#5723,#3829,.T.);
#7454=EDGE_CURVE('',#5722,#5724,#3830,.T.);
#7455=EDGE_CURVE('',#5725,#5724,#3831,.T.);
#7456=EDGE_CURVE('',#5723,#5725,#3832,.T.);
#7457=EDGE_CURVE('',#5723,#5726,#1717,.T.);
#7458=EDGE_CURVE('',#5725,#5726,#3833,.T.);
#7459=EDGE_CURVE('',#5726,#5727,#3834,.T.);
#7460=EDGE_CURVE('',#5724,#5727,#3835,.T.);
#7461=EDGE_CURVE('',#5727,#5722,#1718,.T.);
#7462=EDGE_CURVE('',#5728,#5729,#3836,.T.);
#7463=EDGE_CURVE('',#5728,#5730,#3837,.T.);
#7464=EDGE_CURVE('',#5731,#5730,#3838,.T.);
#7465=EDGE_CURVE('',#5729,#5731,#3839,.T.);
#7466=EDGE_CURVE('',#5729,#5732,#1719,.T.);
#7467=EDGE_CURVE('',#5731,#5732,#3840,.T.);
#7468=EDGE_CURVE('',#5732,#5733,#3841,.T.);
#7469=EDGE_CURVE('',#5730,#5733,#3842,.T.);
#7470=EDGE_CURVE('',#5733,#5728,#1720,.T.);
#7471=EDGE_CURVE('',#5734,#5735,#3843,.T.);
#7472=EDGE_CURVE('',#5734,#5736,#3844,.T.);
#7473=EDGE_CURVE('',#5737,#5736,#3845,.T.);
#7474=EDGE_CURVE('',#5735,#5737,#3846,.T.);
#7475=EDGE_CURVE('',#5735,#5738,#1721,.T.);
#7476=EDGE_CURVE('',#5737,#5738,#3847,.T.);
#7477=EDGE_CURVE('',#5738,#5739,#3848,.T.);
#7478=EDGE_CURVE('',#5736,#5739,#3849,.T.);
#7479=EDGE_CURVE('',#5739,#5734,#1722,.T.);
#7480=EDGE_CURVE('',#5740,#5741,#3850,.T.);
#7481=EDGE_CURVE('',#5740,#5742,#3851,.T.);
#7482=EDGE_CURVE('',#5743,#5742,#3852,.T.);
#7483=EDGE_CURVE('',#5741,#5743,#3853,.T.);
#7484=EDGE_CURVE('',#5741,#5744,#1723,.T.);
#7485=EDGE_CURVE('',#5743,#5744,#3854,.T.);
#7486=EDGE_CURVE('',#5744,#5745,#3855,.T.);
#7487=EDGE_CURVE('',#5742,#5745,#3856,.T.);
#7488=EDGE_CURVE('',#5745,#5740,#1724,.T.);
#7489=EDGE_CURVE('',#5746,#5747,#3857,.T.);
#7490=EDGE_CURVE('',#5746,#5748,#3858,.T.);
#7491=EDGE_CURVE('',#5749,#5748,#3859,.T.);
#7492=EDGE_CURVE('',#5747,#5749,#3860,.T.);
#7493=EDGE_CURVE('',#5747,#5750,#1725,.T.);
#7494=EDGE_CURVE('',#5749,#5750,#3861,.T.);
#7495=EDGE_CURVE('',#5750,#5751,#3862,.T.);
#7496=EDGE_CURVE('',#5748,#5751,#3863,.T.);
#7497=EDGE_CURVE('',#5751,#5746,#1726,.T.);
#7498=EDGE_CURVE('',#5752,#5753,#3864,.T.);
#7499=EDGE_CURVE('',#5752,#5754,#3865,.T.);
#7500=EDGE_CURVE('',#5755,#5754,#3866,.T.);
#7501=EDGE_CURVE('',#5753,#5755,#3867,.T.);
#7502=EDGE_CURVE('',#5753,#5756,#1727,.T.);
#7503=EDGE_CURVE('',#5755,#5756,#3868,.T.);
#7504=EDGE_CURVE('',#5756,#5757,#3869,.T.);
#7505=EDGE_CURVE('',#5754,#5757,#3870,.T.);
#7506=EDGE_CURVE('',#5757,#5752,#1728,.T.);
#7507=EDGE_CURVE('',#5758,#5759,#1729,.T.);
#7508=EDGE_CURVE('',#5758,#5760,#3871,.T.);
#7509=EDGE_CURVE('',#5760,#5759,#3872,.T.);
#7510=EDGE_CURVE('',#5761,#5758,#3873,.T.);
#7511=EDGE_CURVE('',#5761,#5762,#3874,.T.);
#7512=EDGE_CURVE('',#5760,#5762,#3875,.T.);
#7513=EDGE_CURVE('',#5759,#5763,#3876,.T.);
#7514=EDGE_CURVE('',#5762,#5763,#3877,.T.);
#7515=EDGE_CURVE('',#5763,#5761,#1730,.T.);
#7516=EDGE_CURVE('',#5764,#5765,#3878,.T.);
#7517=EDGE_CURVE('',#5764,#5766,#3879,.T.);
#7518=EDGE_CURVE('',#5767,#5766,#3880,.T.);
#7519=EDGE_CURVE('',#5765,#5767,#3881,.T.);
#7520=EDGE_CURVE('',#5765,#5768,#1731,.T.);
#7521=EDGE_CURVE('',#5767,#5768,#3882,.T.);
#7522=EDGE_CURVE('',#5768,#5769,#3883,.T.);
#7523=EDGE_CURVE('',#5766,#5769,#3884,.T.);
#7524=EDGE_CURVE('',#5769,#5764,#1732,.T.);
#7525=EDGE_CURVE('',#5770,#5771,#3885,.T.);
#7526=EDGE_CURVE('',#5770,#5772,#3886,.T.);
#7527=EDGE_CURVE('',#5773,#5772,#3887,.T.);
#7528=EDGE_CURVE('',#5771,#5773,#3888,.T.);
#7529=EDGE_CURVE('',#5771,#5774,#1733,.T.);
#7530=EDGE_CURVE('',#5773,#5774,#3889,.T.);
#7531=EDGE_CURVE('',#5774,#5775,#3890,.T.);
#7532=EDGE_CURVE('',#5772,#5775,#3891,.T.);
#7533=EDGE_CURVE('',#5775,#5770,#1734,.T.);
#7534=EDGE_CURVE('',#5776,#5777,#3892,.T.);
#7535=EDGE_CURVE('',#5776,#5778,#3893,.T.);
#7536=EDGE_CURVE('',#5779,#5778,#3894,.T.);
#7537=EDGE_CURVE('',#5777,#5779,#3895,.T.);
#7538=EDGE_CURVE('',#5777,#5780,#1735,.T.);
#7539=EDGE_CURVE('',#5779,#5780,#3896,.T.);
#7540=EDGE_CURVE('',#5780,#5781,#3897,.T.);
#7541=EDGE_CURVE('',#5778,#5781,#3898,.T.);
#7542=EDGE_CURVE('',#5781,#5776,#1736,.T.);
#7543=EDGE_CURVE('',#5782,#5783,#3899,.T.);
#7544=EDGE_CURVE('',#5782,#5784,#3900,.T.);
#7545=EDGE_CURVE('',#5785,#5784,#3901,.T.);
#7546=EDGE_CURVE('',#5783,#5785,#3902,.T.);
#7547=EDGE_CURVE('',#5783,#5786,#1737,.T.);
#7548=EDGE_CURVE('',#5785,#5786,#3903,.T.);
#7549=EDGE_CURVE('',#5786,#5787,#3904,.T.);
#7550=EDGE_CURVE('',#5784,#5787,#3905,.T.);
#7551=EDGE_CURVE('',#5787,#5782,#1738,.T.);
#7552=EDGE_CURVE('',#5788,#5789,#3906,.T.);
#7553=EDGE_CURVE('',#5788,#5790,#3907,.T.);
#7554=EDGE_CURVE('',#5791,#5790,#3908,.T.);
#7555=EDGE_CURVE('',#5789,#5791,#3909,.T.);
#7556=EDGE_CURVE('',#5789,#5792,#1739,.T.);
#7557=EDGE_CURVE('',#5791,#5792,#3910,.T.);
#7558=EDGE_CURVE('',#5792,#5793,#3911,.T.);
#7559=EDGE_CURVE('',#5790,#5793,#3912,.T.);
#7560=EDGE_CURVE('',#5793,#5788,#1740,.T.);
#7561=EDGE_CURVE('',#5794,#5795,#3913,.T.);
#7562=EDGE_CURVE('',#5794,#5796,#3914,.T.);
#7563=EDGE_CURVE('',#5797,#5796,#3915,.T.);
#7564=EDGE_CURVE('',#5795,#5797,#3916,.T.);
#7565=EDGE_CURVE('',#5795,#5798,#1741,.T.);
#7566=EDGE_CURVE('',#5797,#5798,#3917,.T.);
#7567=EDGE_CURVE('',#5798,#5799,#3918,.T.);
#7568=EDGE_CURVE('',#5796,#5799,#3919,.T.);
#7569=EDGE_CURVE('',#5799,#5794,#1742,.T.);
#7570=EDGE_CURVE('',#5800,#5801,#3920,.T.);
#7571=EDGE_CURVE('',#5800,#5802,#3921,.T.);
#7572=EDGE_CURVE('',#5803,#5802,#3922,.T.);
#7573=EDGE_CURVE('',#5801,#5803,#3923,.T.);
#7574=EDGE_CURVE('',#5801,#5804,#1743,.T.);
#7575=EDGE_CURVE('',#5803,#5804,#3924,.T.);
#7576=EDGE_CURVE('',#5804,#5805,#3925,.T.);
#7577=EDGE_CURVE('',#5802,#5805,#3926,.T.);
#7578=EDGE_CURVE('',#5805,#5800,#1744,.T.);
#7579=EDGE_CURVE('',#5806,#5807,#3927,.T.);
#7580=EDGE_CURVE('',#5806,#5808,#3928,.T.);
#7581=EDGE_CURVE('',#5809,#5808,#3929,.T.);
#7582=EDGE_CURVE('',#5807,#5809,#3930,.T.);
#7583=EDGE_CURVE('',#5807,#5810,#1745,.T.);
#7584=EDGE_CURVE('',#5809,#5810,#3931,.T.);
#7585=EDGE_CURVE('',#5810,#5811,#3932,.T.);
#7586=EDGE_CURVE('',#5808,#5811,#3933,.T.);
#7587=EDGE_CURVE('',#5811,#5806,#1746,.T.);
#7588=EDGE_CURVE('',#5812,#5813,#3934,.T.);
#7589=EDGE_CURVE('',#5812,#5814,#3935,.T.);
#7590=EDGE_CURVE('',#5815,#5814,#3936,.T.);
#7591=EDGE_CURVE('',#5813,#5815,#3937,.T.);
#7592=EDGE_CURVE('',#5813,#5816,#1747,.T.);
#7593=EDGE_CURVE('',#5815,#5816,#3938,.T.);
#7594=EDGE_CURVE('',#5816,#5817,#3939,.T.);
#7595=EDGE_CURVE('',#5814,#5817,#3940,.T.);
#7596=EDGE_CURVE('',#5817,#5812,#1748,.T.);
#7597=EDGE_CURVE('',#5818,#5818,#1749,.T.);
#7598=EDGE_CURVE('',#5818,#5819,#1750,.T.);
#7599=EDGE_CURVE('',#5819,#5819,#1751,.T.);
#7600=EDGE_CURVE('',#5818,#5820,#3941,.T.);
#7601=EDGE_CURVE('',#5820,#5820,#1752,.T.);
#7602=EDGE_CURVE('',#5821,#5821,#1753,.T.);
#7603=EDGE_CURVE('',#5822,#5822,#1754,.T.);
#7604=EDGE_CURVE('',#5583,#5822,#3942,.T.);
#7605=EDGE_CURVE('',#5585,#5581,#1755,.F.);
#7606=EDGE_CURVE('',#5823,#5823,#1756,.T.);
#7607=EDGE_CURVE('',#5823,#5821,#3943,.T.);
#7608=EDGE_CURVE('',#5810,#5601,#1757,.T.);
#7609=EDGE_CURVE('',#5610,#5807,#1758,.T.);
#7610=EDGE_CURVE('',#5804,#5607,#1759,.T.);
#7611=EDGE_CURVE('',#5616,#5801,#1760,.T.);
#7612=EDGE_CURVE('',#5798,#5613,#1761,.T.);
#7613=EDGE_CURVE('',#5622,#5795,#1762,.T.);
#7614=EDGE_CURVE('',#5792,#5619,#1763,.T.);
#7615=EDGE_CURVE('',#5628,#5789,#1764,.T.);
#7616=EDGE_CURVE('',#5786,#5625,#1765,.T.);
#7617=EDGE_CURVE('',#5634,#5783,#1766,.T.);
#7618=EDGE_CURVE('',#5780,#5631,#1767,.T.);
#7619=EDGE_CURVE('',#5640,#5777,#1768,.T.);
#7620=EDGE_CURVE('',#5774,#5637,#1769,.T.);
#7621=EDGE_CURVE('',#5646,#5771,#1770,.T.);
#7622=EDGE_CURVE('',#5768,#5643,#1771,.T.);
#7623=EDGE_CURVE('',#5653,#5765,#1772,.T.);
#7624=EDGE_CURVE('',#5655,#5823,#3944,.T.);
#7625=EDGE_CURVE('',#5660,#5649,#1773,.T.);
#7626=EDGE_CURVE('',#5756,#5657,#1774,.T.);
#7627=EDGE_CURVE('',#5666,#5753,#1775,.T.);
#7628=EDGE_CURVE('',#5750,#5663,#1776,.T.);
#7629=EDGE_CURVE('',#5672,#5747,#1777,.T.);
#7630=EDGE_CURVE('',#5744,#5669,#1778,.T.);
#7631=EDGE_CURVE('',#5678,#5741,#1779,.T.);
#7632=EDGE_CURVE('',#5738,#5675,#1780,.T.);
#7633=EDGE_CURVE('',#5684,#5735,#1781,.T.);
#7634=EDGE_CURVE('',#5732,#5681,#1782,.T.);
#7635=EDGE_CURVE('',#5690,#5729,#1783,.T.);
#7636=EDGE_CURVE('',#5726,#5687,#1784,.T.);
#7637=EDGE_CURVE('',#5696,#5723,#1785,.T.);
#7638=EDGE_CURVE('',#5720,#5693,#1786,.T.);
#7639=EDGE_CURVE('',#5702,#5717,#1787,.T.);
#7640=EDGE_CURVE('',#5714,#5699,#1788,.T.);
#7641=EDGE_CURVE('',#5708,#5711,#1789,.T.);
#7642=EDGE_CURVE('',#5759,#5705,#1790,.T.);
#7643=EDGE_CURVE('',#5816,#5758,#1791,.T.);
#7644=EDGE_CURVE('',#5604,#5813,#1792,.T.);
#7645=EDGE_CURVE('',#5824,#5824,#1793,.T.);
#7646=EDGE_CURVE('',#5824,#5652,#3945,.T.);
#7647=EDGE_CURVE('',#5825,#5825,#1794,.T.);
#7648=EDGE_CURVE('',#5825,#5826,#3946,.T.);
#7649=EDGE_CURVE('',#5826,#5827,#1795,.T.);
#7650=EDGE_CURVE('',#5827,#5826,#1796,.T.);
#7651=EDGE_CURVE('',#5828,#5828,#1797,.T.);
#7652=EDGE_CURVE('',#5827,#5829,#3947,.T.);
#7653=EDGE_CURVE('',#5829,#5829,#1798,.T.);
#7654=EDGE_CURVE('',#5830,#5830,#1799,.T.);
#7655=EDGE_CURVE('',#5830,#5831,#3948,.T.);
#7656=EDGE_CURVE('',#5831,#5832,#1800,.T.);
#7657=EDGE_CURVE('',#5832,#5831,#1801,.T.);
#7658=EDGE_CURVE('',#5833,#5834,#1802,.T.);
#7659=EDGE_CURVE('',#5834,#5833,#1803,.T.);
#7660=EDGE_CURVE('',#5834,#5832,#3949,.T.);
#7661=EDGE_CURVE('',#5835,#5835,#1804,.T.);
#7662=EDGE_CURVE('',#5833,#5828,#3950,.T.);
#7663=EDGE_CURVE('',#5829,#5835,#3951,.T.);
#7664=EDGE_CURVE('',#5836,#5837,#3952,.T.);
#7665=EDGE_CURVE('',#5838,#5836,#1149,.F.);
#7666=EDGE_CURVE('',#5837,#5838,#1150,.F.);
#7667=EDGE_CURVE('',#5839,#5840,#1151,.F.);
#7668=EDGE_CURVE('',#5841,#5839,#1152,.F.);
#7669=EDGE_CURVE('',#5840,#5841,#3953,.T.);
#7670=EDGE_CURVE('',#5842,#5843,#3954,.T.);
#7671=EDGE_CURVE('',#5844,#5842,#1153,.F.);
#7672=EDGE_CURVE('',#5843,#5844,#1154,.F.);
#7673=EDGE_CURVE('',#5845,#5846,#1155,.F.);
#7674=EDGE_CURVE('',#5847,#5845,#1156,.F.);
#7675=EDGE_CURVE('',#5846,#5847,#3955,.T.);
#7676=EDGE_CURVE('',#5848,#5849,#3956,.T.);
#7677=EDGE_CURVE('',#5850,#5848,#1157,.F.);
#7678=EDGE_CURVE('',#5849,#5850,#1158,.F.);
#7679=EDGE_CURVE('',#5851,#5852,#1159,.F.);
#7680=EDGE_CURVE('',#5853,#5851,#1160,.F.);
#7681=EDGE_CURVE('',#5852,#5853,#3957,.T.);
#7682=EDGE_CURVE('',#5854,#5855,#1161,.T.);
#7683=EDGE_CURVE('',#5855,#5850,#1162,.T.);
#7684=EDGE_CURVE('',#5848,#5853,#1163,.T.);
#7685=EDGE_CURVE('',#5851,#5854,#1164,.T.);
#7686=EDGE_CURVE('',#5856,#5857,#159,.T.);
#7687=EDGE_CURVE('',#5857,#5852,#3958,.T.);
#7688=EDGE_CURVE('',#5853,#5856,#3959,.T.);
#7689=EDGE_CURVE('',#5858,#5859,#1165,.T.);
#7690=EDGE_CURVE('',#5859,#5851,#1166,.T.);
#7691=EDGE_CURVE('',#5852,#5847,#1167,.T.);
#7692=EDGE_CURVE('',#5845,#5858,#1168,.T.);
#7693=EDGE_CURVE('',#5860,#5861,#1169,.T.);
#7694=EDGE_CURVE('',#5861,#5844,#1170,.T.);
#7695=EDGE_CURVE('',#5842,#5849,#1171,.T.);
#7696=EDGE_CURVE('',#5850,#5860,#1172,.T.);
#7697=EDGE_CURVE('',#5862,#5863,#160,.T.);
#7698=EDGE_CURVE('',#5863,#5848,#3960,.T.);
#7699=EDGE_CURVE('',#5849,#5862,#3961,.T.);
#7700=EDGE_CURVE('',#5864,#5865,#161,.T.);
#7701=EDGE_CURVE('',#5865,#5846,#3962,.T.);
#7702=EDGE_CURVE('',#5847,#5864,#3963,.T.);
#7703=EDGE_CURVE('',#5866,#5867,#1173,.T.);
#7704=EDGE_CURVE('',#5867,#5845,#1174,.T.);
#7705=EDGE_CURVE('',#5846,#5841,#1175,.T.);
#7706=EDGE_CURVE('',#5839,#5866,#1176,.T.);
#7707=EDGE_CURVE('',#5868,#5869,#1177,.T.);
#7708=EDGE_CURVE('',#5869,#5870,#1178,.T.);
#7709=EDGE_CURVE('',#5870,#5838,#1179,.T.);
#7710=EDGE_CURVE('',#5836,#5843,#1180,.T.);
#7711=EDGE_CURVE('',#5844,#5868,#1181,.T.);
#7712=EDGE_CURVE('',#5871,#5872,#162,.T.);
#7713=EDGE_CURVE('',#5872,#5842,#3964,.T.);
#7714=EDGE_CURVE('',#5843,#5871,#3965,.T.);
#7715=EDGE_CURVE('',#5873,#5874,#163,.T.);
#7716=EDGE_CURVE('',#5874,#5840,#3966,.T.);
#7717=EDGE_CURVE('',#5841,#5873,#3967,.T.);
#7718=EDGE_CURVE('',#5875,#5876,#1182,.T.);
#7719=EDGE_CURVE('',#5876,#5839,#1183,.T.);
#7720=EDGE_CURVE('',#5840,#5837,#1184,.T.);
#7721=EDGE_CURVE('',#5838,#5875,#1185,.T.);
#7722=EDGE_CURVE('',#5877,#5878,#164,.T.);
#7723=EDGE_CURVE('',#5878,#5836,#3968,.T.);
#7724=EDGE_CURVE('',#5837,#5877,#3969,.T.);
#7725=EDGE_CURVE('',#5872,#5862,#165,.T.);
#7726=EDGE_CURVE('',#5878,#5871,#166,.T.);
#7727=EDGE_CURVE('',#5874,#5877,#167,.T.);
#7728=EDGE_CURVE('',#5879,#5879,#1805,.T.);
#7729=EDGE_CURVE('',#5879,#5880,#3970,.T.);
#7730=EDGE_CURVE('',#5857,#5880,#168,.T.);
#7731=EDGE_CURVE('',#5863,#5856,#169,.T.);
#7732=EDGE_CURVE('',#5865,#5873,#170,.T.);
#7733=EDGE_CURVE('',#5880,#5864,#171,.T.);
#7734=EDGE_CURVE('',#5858,#5867,#1806,.T.);
#7735=EDGE_CURVE('',#5866,#5876,#1807,.T.);
#7736=EDGE_CURVE('',#5875,#5870,#1808,.T.);
#7737=EDGE_CURVE('',#5868,#5861,#1809,.T.);
#7738=EDGE_CURVE('',#5860,#5855,#1810,.T.);
#7739=EDGE_CURVE('',#5854,#5859,#1811,.T.);
#7740=EDGE_CURVE('',#5881,#5881,#1812,.T.);
#7741=EDGE_CURVE('',#5881,#5869,#3971,.T.);
#7742=EDGE_CURVE('',#5882,#5882,#1813,.T.);
#7743=EDGE_CURVE('',#5883,#5883,#1814,.T.);
#7744=EDGE_CURVE('',#5883,#5882,#3972,.T.);
#7745=EDGE_CURVE('',#5883,#5884,#3973,.T.);
#7746=EDGE_CURVE('',#5884,#5884,#1815,.T.);
#7747=EDGE_CURVE('',#5884,#5885,#3974,.T.);
#7748=EDGE_CURVE('',#5885,#5885,#1816,.T.);
#7749=EDGE_CURVE('',#5885,#5886,#3975,.T.);
#7750=EDGE_CURVE('',#5886,#5886,#1817,.T.);
#7751=EDGE_CURVE('',#5886,#5887,#3976,.T.);
#7752=EDGE_CURVE('',#5887,#5887,#1818,.T.);
#7753=ORIENTED_EDGE('',*,*,#5888,.T.);
#7754=ORIENTED_EDGE('',*,*,#5889,.T.);
#7755=ORIENTED_EDGE('',*,*,#5890,.T.);
#7756=ORIENTED_EDGE('',*,*,#5891,.T.);
#7757=ORIENTED_EDGE('',*,*,#5892,.T.);
#7758=ORIENTED_EDGE('',*,*,#5893,.T.);
#7759=ORIENTED_EDGE('',*,*,#5892,.F.);
#7760=ORIENTED_EDGE('',*,*,#5894,.F.);
#7761=ORIENTED_EDGE('',*,*,#5895,.F.);
#7762=ORIENTED_EDGE('',*,*,#5896,.F.);
#7763=ORIENTED_EDGE('',*,*,#5897,.F.);
#7764=ORIENTED_EDGE('',*,*,#5898,.F.);
#7765=ORIENTED_EDGE('',*,*,#5899,.T.);
#7766=ORIENTED_EDGE('',*,*,#5891,.F.);
#7767=ORIENTED_EDGE('',*,*,#5900,.T.);
#7768=ORIENTED_EDGE('',*,*,#5901,.F.);
#7769=ORIENTED_EDGE('',*,*,#5902,.T.);
#7770=ORIENTED_EDGE('',*,*,#5894,.T.);
#7771=ORIENTED_EDGE('',*,*,#5890,.F.);
#7772=ORIENTED_EDGE('',*,*,#5903,.F.);
#7773=ORIENTED_EDGE('',*,*,#5904,.F.);
#7774=ORIENTED_EDGE('',*,*,#5905,.F.);
#7775=ORIENTED_EDGE('',*,*,#5906,.F.);
#7776=ORIENTED_EDGE('',*,*,#5907,.F.);
#7777=ORIENTED_EDGE('',*,*,#5900,.F.);
#7778=ORIENTED_EDGE('',*,*,#5904,.T.);
#7779=ORIENTED_EDGE('',*,*,#5908,.T.);
#7780=ORIENTED_EDGE('',*,*,#5909,.T.);
#7781=ORIENTED_EDGE('',*,*,#5910,.T.);
#7782=ORIENTED_EDGE('',*,*,#5911,.T.);
#7783=ORIENTED_EDGE('',*,*,#5912,.T.);
#7784=ORIENTED_EDGE('',*,*,#5911,.F.);
#7785=ORIENTED_EDGE('',*,*,#5913,.F.);
#7786=ORIENTED_EDGE('',*,*,#5914,.F.);
#7787=ORIENTED_EDGE('',*,*,#5915,.F.);
#7788=ORIENTED_EDGE('',*,*,#5910,.F.);
#7789=ORIENTED_EDGE('',*,*,#5916,.T.);
#7790=ORIENTED_EDGE('',*,*,#5917,.F.);
#7791=ORIENTED_EDGE('',*,*,#5918,.T.);
#7792=ORIENTED_EDGE('',*,*,#5919,.F.);
#7793=ORIENTED_EDGE('',*,*,#5913,.T.);
#7794=ORIENTED_EDGE('',*,*,#5888,.F.);
#7795=ORIENTED_EDGE('',*,*,#5920,.F.);
#7796=ORIENTED_EDGE('',*,*,#5921,.F.);
#7797=ORIENTED_EDGE('',*,*,#5922,.F.);
#7798=ORIENTED_EDGE('',*,*,#5916,.F.);
#7799=ORIENTED_EDGE('',*,*,#5909,.F.);
#7800=ORIENTED_EDGE('',*,*,#5923,.F.);
#7801=ORIENTED_EDGE('',*,*,#5924,.T.);
#7802=ORIENTED_EDGE('',*,*,#5925,.T.);
#7803=ORIENTED_EDGE('',*,*,#5926,.T.);
#7804=ORIENTED_EDGE('',*,*,#5927,.T.);
#7805=ORIENTED_EDGE('',*,*,#5914,.T.);
#7806=ORIENTED_EDGE('',*,*,#5919,.T.);
#7807=ORIENTED_EDGE('',*,*,#5912,.F.);
#7808=ORIENTED_EDGE('',*,*,#5915,.T.);
#7809=ORIENTED_EDGE('',*,*,#5927,.F.);
#7810=ORIENTED_EDGE('',*,*,#5928,.T.);
#7811=ORIENTED_EDGE('',*,*,#5929,.F.);
#7812=ORIENTED_EDGE('',*,*,#5905,.T.);
#7813=ORIENTED_EDGE('',*,*,#5926,.F.);
#7814=ORIENTED_EDGE('',*,*,#5930,.F.);
#7815=ORIENTED_EDGE('',*,*,#5931,.F.);
#7816=ORIENTED_EDGE('',*,*,#5932,.F.);
#7817=ORIENTED_EDGE('',*,*,#5933,.F.);
#7818=ORIENTED_EDGE('',*,*,#5934,.F.);
#7819=ORIENTED_EDGE('',*,*,#5928,.F.);
#7820=ORIENTED_EDGE('',*,*,#5931,.T.);
#7821=ORIENTED_EDGE('',*,*,#5935,.T.);
#7822=ORIENTED_EDGE('',*,*,#5936,.T.);
#7823=ORIENTED_EDGE('',*,*,#5937,.T.);
#7824=ORIENTED_EDGE('',*,*,#5938,.T.);
#7825=ORIENTED_EDGE('',*,*,#5939,.T.);
#7826=ORIENTED_EDGE('',*,*,#5938,.F.);
#7827=ORIENTED_EDGE('',*,*,#5940,.F.);
#7828=ORIENTED_EDGE('',*,*,#5941,.F.);
#7829=ORIENTED_EDGE('',*,*,#5942,.F.);
#7830=ORIENTED_EDGE('',*,*,#5943,.T.);
#7831=ORIENTED_EDGE('',*,*,#5937,.F.);
#7832=ORIENTED_EDGE('',*,*,#5944,.T.);
#7833=ORIENTED_EDGE('',*,*,#5945,.F.);
#7834=ORIENTED_EDGE('',*,*,#5946,.T.);
#7835=ORIENTED_EDGE('',*,*,#5947,.F.);
#7836=ORIENTED_EDGE('',*,*,#5940,.T.);
#7837=ORIENTED_EDGE('',*,*,#5924,.F.);
#7838=ORIENTED_EDGE('',*,*,#5918,.F.);
#7839=ORIENTED_EDGE('',*,*,#5948,.F.);
#7840=ORIENTED_EDGE('',*,*,#5949,.F.);
#7841=ORIENTED_EDGE('',*,*,#5944,.F.);
#7842=ORIENTED_EDGE('',*,*,#5936,.F.);
#7843=ORIENTED_EDGE('',*,*,#5950,.F.);
#7844=ORIENTED_EDGE('',*,*,#5951,.T.);
#7845=ORIENTED_EDGE('',*,*,#5952,.T.);
#7846=ORIENTED_EDGE('',*,*,#5953,.T.);
#7847=ORIENTED_EDGE('',*,*,#5954,.T.);
#7848=ORIENTED_EDGE('',*,*,#5941,.T.);
#7849=ORIENTED_EDGE('',*,*,#5947,.T.);
#7850=ORIENTED_EDGE('',*,*,#5939,.F.);
#7851=ORIENTED_EDGE('',*,*,#5942,.T.);
#7852=ORIENTED_EDGE('',*,*,#5954,.F.);
#7853=ORIENTED_EDGE('',*,*,#5955,.T.);
#7854=ORIENTED_EDGE('',*,*,#5956,.F.);
#7855=ORIENTED_EDGE('',*,*,#5932,.T.);
#7856=ORIENTED_EDGE('',*,*,#5953,.F.);
#7857=ORIENTED_EDGE('',*,*,#5957,.F.);
#7858=ORIENTED_EDGE('',*,*,#5958,.F.);
#7859=ORIENTED_EDGE('',*,*,#5959,.F.);
#7860=ORIENTED_EDGE('',*,*,#5960,.F.);
#7861=ORIENTED_EDGE('',*,*,#5961,.F.);
#7862=ORIENTED_EDGE('',*,*,#5955,.F.);
#7863=ORIENTED_EDGE('',*,*,#5952,.F.);
#7864=ORIENTED_EDGE('',*,*,#5962,.T.);
#7865=ORIENTED_EDGE('',*,*,#5963,.F.);
#7866=ORIENTED_EDGE('',*,*,#5957,.T.);
#7867=ORIENTED_EDGE('',*,*,#5958,.T.);
#7868=ORIENTED_EDGE('',*,*,#5963,.T.);
#7869=ORIENTED_EDGE('',*,*,#5964,.T.);
#7870=ORIENTED_EDGE('',*,*,#5965,.T.);
#7871=ORIENTED_EDGE('',*,*,#5966,.T.);
#7872=ORIENTED_EDGE('',*,*,#5967,.T.);
#7873=ORIENTED_EDGE('',*,*,#5967,.F.);
#7874=ORIENTED_EDGE('',*,*,#5968,.T.);
#7875=ORIENTED_EDGE('',*,*,#5969,.F.);
#7876=ORIENTED_EDGE('',*,*,#5970,.T.);
#7877=ORIENTED_EDGE('',*,*,#5971,.F.);
#7878=ORIENTED_EDGE('',*,*,#5959,.T.);
#7879=ORIENTED_EDGE('',*,*,#5972,.T.);
#7880=ORIENTED_EDGE('',*,*,#5973,.T.);
#7881=ORIENTED_EDGE('',*,*,#5974,.T.);
#7882=ORIENTED_EDGE('',*,*,#5975,.T.);
#7883=ORIENTED_EDGE('',*,*,#5976,.T.);
#7884=ORIENTED_EDGE('',*,*,#5977,.T.);
#7885=ORIENTED_EDGE('',*,*,#5972,.F.);
#7886=ORIENTED_EDGE('',*,*,#5978,.F.);
#7887=ORIENTED_EDGE('',*,*,#5979,.F.);
#7888=ORIENTED_EDGE('',*,*,#5980,.F.);
#7889=ORIENTED_EDGE('',*,*,#5970,.F.);
#7890=ORIENTED_EDGE('',*,*,#5981,.F.);
#7891=ORIENTED_EDGE('',*,*,#5982,.F.);
#7892=ORIENTED_EDGE('',*,*,#5977,.F.);
#7893=ORIENTED_EDGE('',*,*,#5983,.T.);
#7894=ORIENTED_EDGE('',*,*,#5984,.F.);
#7895=ORIENTED_EDGE('',*,*,#5985,.T.);
#7896=ORIENTED_EDGE('',*,*,#5986,.F.);
#7897=ORIENTED_EDGE('',*,*,#5978,.T.);
#7898=ORIENTED_EDGE('',*,*,#5976,.F.);
#7899=ORIENTED_EDGE('',*,*,#5987,.F.);
#7900=ORIENTED_EDGE('',*,*,#5988,.F.);
#7901=ORIENTED_EDGE('',*,*,#5983,.F.);
#7902=ORIENTED_EDGE('',*,*,#5989,.T.);
#7903=ORIENTED_EDGE('',*,*,#5990,.T.);
#7904=ORIENTED_EDGE('',*,*,#5991,.T.);
#7905=ORIENTED_EDGE('',*,*,#5981,.T.);
#7906=ORIENTED_EDGE('',*,*,#5969,.T.);
#7907=ORIENTED_EDGE('',*,*,#5992,.T.);
#7908=ORIENTED_EDGE('',*,*,#5993,.T.);
#7909=ORIENTED_EDGE('',*,*,#5973,.F.);
#7910=ORIENTED_EDGE('',*,*,#5982,.T.);
#7911=ORIENTED_EDGE('',*,*,#5991,.F.);
#7912=ORIENTED_EDGE('',*,*,#5994,.T.);
#7913=ORIENTED_EDGE('',*,*,#5974,.F.);
#7914=ORIENTED_EDGE('',*,*,#5994,.F.);
#7915=ORIENTED_EDGE('',*,*,#5990,.F.);
#7916=ORIENTED_EDGE('',*,*,#5995,.F.);
#7917=ORIENTED_EDGE('',*,*,#5996,.F.);
#7918=ORIENTED_EDGE('',*,*,#5997,.F.);
#7919=ORIENTED_EDGE('',*,*,#5998,.F.);
#7920=ORIENTED_EDGE('',*,*,#5965,.F.);
#7921=ORIENTED_EDGE('',*,*,#5999,.T.);
#7922=ORIENTED_EDGE('',*,*,#6000,.F.);
#7923=ORIENTED_EDGE('',*,*,#5995,.T.);
#7924=ORIENTED_EDGE('',*,*,#5993,.F.);
#7925=ORIENTED_EDGE('',*,*,#6001,.T.);
#7926=ORIENTED_EDGE('',*,*,#6002,.T.);
#7927=ORIENTED_EDGE('',*,*,#6003,.T.);
#7928=ORIENTED_EDGE('',*,*,#6004,.T.);
#7929=ORIENTED_EDGE('',*,*,#5984,.T.);
#7930=ORIENTED_EDGE('',*,*,#5988,.T.);
#7931=ORIENTED_EDGE('',*,*,#6005,.T.);
#7932=ORIENTED_EDGE('',*,*,#6004,.F.);
#7933=ORIENTED_EDGE('',*,*,#6006,.F.);
#7934=ORIENTED_EDGE('',*,*,#6007,.F.);
#7935=ORIENTED_EDGE('',*,*,#6008,.F.);
#7936=ORIENTED_EDGE('',*,*,#6009,.F.);
#7937=ORIENTED_EDGE('',*,*,#6010,.F.);
#7938=ORIENTED_EDGE('',*,*,#5985,.F.);
#7939=ORIENTED_EDGE('',*,*,#6007,.T.);
#7940=ORIENTED_EDGE('',*,*,#6011,.T.);
#7941=ORIENTED_EDGE('',*,*,#6012,.T.);
#7942=ORIENTED_EDGE('',*,*,#6013,.T.);
#7943=ORIENTED_EDGE('',*,*,#6014,.T.);
#7944=ORIENTED_EDGE('',*,*,#6015,.T.);
#7945=ORIENTED_EDGE('',*,*,#6014,.F.);
#7946=ORIENTED_EDGE('',*,*,#6016,.F.);
#7947=ORIENTED_EDGE('',*,*,#6017,.F.);
#7948=ORIENTED_EDGE('',*,*,#6018,.F.);
#7949=ORIENTED_EDGE('',*,*,#6013,.F.);
#7950=ORIENTED_EDGE('',*,*,#6019,.T.);
#7951=ORIENTED_EDGE('',*,*,#6020,.F.);
#7952=ORIENTED_EDGE('',*,*,#6021,.T.);
#7953=ORIENTED_EDGE('',*,*,#6022,.F.);
#7954=ORIENTED_EDGE('',*,*,#6016,.T.);
#7955=ORIENTED_EDGE('',*,*,#6002,.F.);
#7956=ORIENTED_EDGE('',*,*,#6023,.F.);
#7957=ORIENTED_EDGE('',*,*,#6024,.F.);
#7958=ORIENTED_EDGE('',*,*,#6025,.F.);
#7959=ORIENTED_EDGE('',*,*,#6019,.F.);
#7960=ORIENTED_EDGE('',*,*,#6012,.F.);
#7961=ORIENTED_EDGE('',*,*,#6026,.F.);
#7962=ORIENTED_EDGE('',*,*,#6027,.T.);
#7963=ORIENTED_EDGE('',*,*,#6028,.T.);
#7964=ORIENTED_EDGE('',*,*,#6029,.T.);
#7965=ORIENTED_EDGE('',*,*,#6030,.T.);
#7966=ORIENTED_EDGE('',*,*,#6017,.T.);
#7967=ORIENTED_EDGE('',*,*,#6022,.T.);
#7968=ORIENTED_EDGE('',*,*,#6015,.F.);
#7969=ORIENTED_EDGE('',*,*,#6018,.T.);
#7970=ORIENTED_EDGE('',*,*,#6030,.F.);
#7971=ORIENTED_EDGE('',*,*,#6031,.T.);
#7972=ORIENTED_EDGE('',*,*,#6032,.F.);
#7973=ORIENTED_EDGE('',*,*,#6008,.T.);
#7974=ORIENTED_EDGE('',*,*,#6029,.F.);
#7975=ORIENTED_EDGE('',*,*,#6033,.F.);
#7976=ORIENTED_EDGE('',*,*,#6034,.F.);
#7977=ORIENTED_EDGE('',*,*,#6035,.F.);
#7978=ORIENTED_EDGE('',*,*,#6036,.F.);
#7979=ORIENTED_EDGE('',*,*,#6037,.F.);
#7980=ORIENTED_EDGE('',*,*,#6031,.F.);
#7981=ORIENTED_EDGE('',*,*,#6034,.T.);
#7982=ORIENTED_EDGE('',*,*,#6038,.T.);
#7983=ORIENTED_EDGE('',*,*,#6039,.T.);
#7984=ORIENTED_EDGE('',*,*,#6040,.T.);
#7985=ORIENTED_EDGE('',*,*,#6041,.T.);
#7986=ORIENTED_EDGE('',*,*,#6042,.T.);
#7987=ORIENTED_EDGE('',*,*,#6041,.F.);
#7988=ORIENTED_EDGE('',*,*,#6043,.F.);
#7989=ORIENTED_EDGE('',*,*,#6044,.F.);
#7990=ORIENTED_EDGE('',*,*,#6045,.F.);
#7991=ORIENTED_EDGE('',*,*,#6046,.F.);
#7992=ORIENTED_EDGE('',*,*,#6047,.F.);
#7993=ORIENTED_EDGE('',*,*,#6048,.T.);
#7994=ORIENTED_EDGE('',*,*,#6040,.F.);
#7995=ORIENTED_EDGE('',*,*,#6049,.T.);
#7996=ORIENTED_EDGE('',*,*,#6050,.F.);
#7997=ORIENTED_EDGE('',*,*,#6051,.T.);
#7998=ORIENTED_EDGE('',*,*,#6043,.T.);
#7999=ORIENTED_EDGE('',*,*,#6027,.F.);
#8000=ORIENTED_EDGE('',*,*,#6021,.F.);
#8001=ORIENTED_EDGE('',*,*,#6052,.F.);
#8002=ORIENTED_EDGE('',*,*,#6053,.F.);
#8003=ORIENTED_EDGE('',*,*,#6049,.F.);
#8004=ORIENTED_EDGE('',*,*,#6039,.F.);
#8005=ORIENTED_EDGE('',*,*,#6054,.F.);
#8006=ORIENTED_EDGE('',*,*,#6009,.T.);
#8007=ORIENTED_EDGE('',*,*,#6032,.T.);
#8008=ORIENTED_EDGE('',*,*,#6037,.T.);
#8009=ORIENTED_EDGE('',*,*,#6055,.T.);
#8010=ORIENTED_EDGE('',*,*,#6056,.T.);
#8011=ORIENTED_EDGE('',*,*,#6057,.T.);
#8012=ORIENTED_EDGE('',*,*,#6055,.F.);
#8013=ORIENTED_EDGE('',*,*,#6036,.T.);
#8014=ORIENTED_EDGE('',*,*,#6058,.T.);
#8015=ORIENTED_EDGE('',*,*,#6059,.F.);
#8016=ORIENTED_EDGE('',*,*,#6060,.T.);
#8017=ORIENTED_EDGE('',*,*,#6061,.T.);
#8018=ORIENTED_EDGE('',*,*,#6062,.T.);
#8019=ORIENTED_EDGE('',*,*,#6059,.T.);
#8020=ORIENTED_EDGE('',*,*,#6063,.T.);
#8021=ORIENTED_EDGE('',*,*,#6061,.F.);
#8022=ORIENTED_EDGE('',*,*,#6064,.T.);
#8023=ORIENTED_EDGE('',*,*,#6065,.T.);
#8024=ORIENTED_EDGE('',*,*,#6056,.F.);
#8025=ORIENTED_EDGE('',*,*,#6060,.F.);
#8026=ORIENTED_EDGE('',*,*,#6062,.F.);
#8027=ORIENTED_EDGE('',*,*,#6065,.F.);
#8028=ORIENTED_EDGE('',*,*,#6066,.F.);
#8029=ORIENTED_EDGE('',*,*,#6067,.F.);
#8030=ORIENTED_EDGE('',*,*,#6068,.F.);
#8031=ORIENTED_EDGE('',*,*,#6069,.F.);
#8032=ORIENTED_EDGE('',*,*,#6070,.F.);
#8033=ORIENTED_EDGE('',*,*,#6071,.F.);
#8034=ORIENTED_EDGE('',*,*,#6072,.F.);
#8035=ORIENTED_EDGE('',*,*,#6073,.F.);
#8036=ORIENTED_EDGE('',*,*,#6074,.F.);
#8037=ORIENTED_EDGE('',*,*,#6075,.F.);
#8038=ORIENTED_EDGE('',*,*,#6076,.F.);
#8039=ORIENTED_EDGE('',*,*,#6077,.F.);
#8040=ORIENTED_EDGE('',*,*,#6078,.F.);
#8041=ORIENTED_EDGE('',*,*,#6079,.F.);
#8042=ORIENTED_EDGE('',*,*,#6080,.F.);
#8043=ORIENTED_EDGE('',*,*,#6081,.F.);
#8044=ORIENTED_EDGE('',*,*,#6064,.F.);
#8045=ORIENTED_EDGE('',*,*,#6063,.F.);
#8046=ORIENTED_EDGE('',*,*,#6082,.F.);
#8047=ORIENTED_EDGE('',*,*,#6083,.T.);
#8048=ORIENTED_EDGE('',*,*,#6084,.F.);
#8049=ORIENTED_EDGE('',*,*,#5960,.T.);
#8050=ORIENTED_EDGE('',*,*,#5971,.T.);
#8051=ORIENTED_EDGE('',*,*,#5980,.T.);
#8052=ORIENTED_EDGE('',*,*,#6085,.T.);
#8053=ORIENTED_EDGE('',*,*,#6076,.T.);
#8054=ORIENTED_EDGE('',*,*,#6086,.T.);
#8055=ORIENTED_EDGE('',*,*,#6057,.F.);
#8056=ORIENTED_EDGE('',*,*,#6077,.T.);
#8057=ORIENTED_EDGE('',*,*,#6085,.F.);
#8058=ORIENTED_EDGE('',*,*,#5979,.T.);
#8059=ORIENTED_EDGE('',*,*,#5986,.T.);
#8060=ORIENTED_EDGE('',*,*,#6010,.T.);
#8061=ORIENTED_EDGE('',*,*,#6087,.T.);
#8062=ORIENTED_EDGE('',*,*,#6074,.T.);
#8063=ORIENTED_EDGE('',*,*,#6088,.T.);
#8064=ORIENTED_EDGE('',*,*,#5906,.T.);
#8065=ORIENTED_EDGE('',*,*,#5929,.T.);
#8066=ORIENTED_EDGE('',*,*,#5934,.T.);
#8067=ORIENTED_EDGE('',*,*,#6086,.F.);
#8068=ORIENTED_EDGE('',*,*,#6075,.T.);
#8069=ORIENTED_EDGE('',*,*,#6087,.F.);
#8070=ORIENTED_EDGE('',*,*,#5933,.T.);
#8071=ORIENTED_EDGE('',*,*,#5956,.T.);
#8072=ORIENTED_EDGE('',*,*,#5961,.T.);
#8073=ORIENTED_EDGE('',*,*,#6088,.F.);
#8074=ORIENTED_EDGE('',*,*,#6073,.T.);
#8075=ORIENTED_EDGE('',*,*,#6089,.T.);
#8076=ORIENTED_EDGE('',*,*,#5901,.T.);
#8077=ORIENTED_EDGE('',*,*,#5907,.T.);
#8078=ORIENTED_EDGE('',*,*,#6090,.T.);
#8079=ORIENTED_EDGE('',*,*,#6091,.T.);
#8080=ORIENTED_EDGE('',*,*,#6089,.F.);
#8081=ORIENTED_EDGE('',*,*,#6072,.T.);
#8082=ORIENTED_EDGE('',*,*,#6090,.F.);
#8083=ORIENTED_EDGE('',*,*,#6071,.T.);
#8084=ORIENTED_EDGE('',*,*,#6092,.T.);
#8085=ORIENTED_EDGE('',*,*,#5948,.T.);
#8086=ORIENTED_EDGE('',*,*,#5917,.T.);
#8087=ORIENTED_EDGE('',*,*,#5922,.T.);
#8088=ORIENTED_EDGE('',*,*,#6093,.T.);
#8089=ORIENTED_EDGE('',*,*,#6094,.T.);
#8090=ORIENTED_EDGE('',*,*,#6095,.T.);
#8091=ORIENTED_EDGE('',*,*,#6093,.F.);
#8092=ORIENTED_EDGE('',*,*,#5921,.T.);
#8093=ORIENTED_EDGE('',*,*,#6096,.T.);
#8094=ORIENTED_EDGE('',*,*,#6097,.F.);
#8095=ORIENTED_EDGE('',*,*,#6098,.T.);
#8096=ORIENTED_EDGE('',*,*,#6099,.T.);
#8097=ORIENTED_EDGE('',*,*,#6100,.T.);
#8098=ORIENTED_EDGE('',*,*,#6097,.T.);
#8099=ORIENTED_EDGE('',*,*,#6101,.T.);
#8100=ORIENTED_EDGE('',*,*,#6099,.F.);
#8101=ORIENTED_EDGE('',*,*,#6102,.T.);
#8102=ORIENTED_EDGE('',*,*,#6103,.T.);
#8103=ORIENTED_EDGE('',*,*,#6094,.F.);
#8104=ORIENTED_EDGE('',*,*,#6098,.F.);
#8105=ORIENTED_EDGE('',*,*,#6100,.F.);
#8106=ORIENTED_EDGE('',*,*,#6103,.F.);
#8107=ORIENTED_EDGE('',*,*,#6104,.F.);
#8108=ORIENTED_EDGE('',*,*,#6105,.F.);
#8109=ORIENTED_EDGE('',*,*,#6106,.F.);
#8110=ORIENTED_EDGE('',*,*,#6107,.F.);
#8111=ORIENTED_EDGE('',*,*,#6108,.F.);
#8112=ORIENTED_EDGE('',*,*,#6109,.F.);
#8113=ORIENTED_EDGE('',*,*,#6110,.F.);
#8114=ORIENTED_EDGE('',*,*,#6111,.F.);
#8115=ORIENTED_EDGE('',*,*,#6112,.F.);
#8116=ORIENTED_EDGE('',*,*,#6113,.F.);
#8117=ORIENTED_EDGE('',*,*,#6114,.F.);
#8118=ORIENTED_EDGE('',*,*,#6115,.F.);
#8119=ORIENTED_EDGE('',*,*,#6116,.F.);
#8120=ORIENTED_EDGE('',*,*,#6117,.F.);
#8121=ORIENTED_EDGE('',*,*,#6118,.F.);
#8122=ORIENTED_EDGE('',*,*,#6119,.F.);
#8123=ORIENTED_EDGE('',*,*,#6102,.F.);
#8124=ORIENTED_EDGE('',*,*,#6101,.F.);
#8125=ORIENTED_EDGE('',*,*,#6120,.F.);
#8126=ORIENTED_EDGE('',*,*,#6121,.T.);
#8127=ORIENTED_EDGE('',*,*,#6122,.F.);
#8128=ORIENTED_EDGE('',*,*,#5996,.T.);
#8129=ORIENTED_EDGE('',*,*,#6000,.T.);
#8130=ORIENTED_EDGE('',*,*,#6123,.T.);
#8131=ORIENTED_EDGE('',*,*,#6124,.T.);
#8132=ORIENTED_EDGE('',*,*,#6114,.T.);
#8133=ORIENTED_EDGE('',*,*,#6125,.T.);
#8134=ORIENTED_EDGE('',*,*,#6095,.F.);
#8135=ORIENTED_EDGE('',*,*,#6115,.T.);
#8136=ORIENTED_EDGE('',*,*,#6124,.F.);
#8137=ORIENTED_EDGE('',*,*,#6126,.T.);
#8138=ORIENTED_EDGE('',*,*,#5945,.T.);
#8139=ORIENTED_EDGE('',*,*,#5949,.T.);
#8140=ORIENTED_EDGE('',*,*,#5951,.F.);
#8141=ORIENTED_EDGE('',*,*,#5946,.F.);
#8142=ORIENTED_EDGE('',*,*,#6126,.F.);
#8143=ORIENTED_EDGE('',*,*,#6123,.F.);
#8144=ORIENTED_EDGE('',*,*,#5999,.F.);
#8145=ORIENTED_EDGE('',*,*,#5964,.F.);
#8146=ORIENTED_EDGE('',*,*,#5962,.F.);
#8147=ORIENTED_EDGE('',*,*,#6127,.T.);
#8148=ORIENTED_EDGE('',*,*,#6112,.T.);
#8149=ORIENTED_EDGE('',*,*,#6128,.T.);
#8150=ORIENTED_EDGE('',*,*,#6052,.T.);
#8151=ORIENTED_EDGE('',*,*,#6020,.T.);
#8152=ORIENTED_EDGE('',*,*,#6025,.T.);
#8153=ORIENTED_EDGE('',*,*,#6125,.F.);
#8154=ORIENTED_EDGE('',*,*,#6113,.T.);
#8155=ORIENTED_EDGE('',*,*,#6127,.F.);
#8156=ORIENTED_EDGE('',*,*,#6024,.T.);
#8157=ORIENTED_EDGE('',*,*,#6129,.T.);
#8158=ORIENTED_EDGE('',*,*,#5997,.T.);
#8159=ORIENTED_EDGE('',*,*,#6128,.F.);
#8160=ORIENTED_EDGE('',*,*,#6111,.T.);
#8161=ORIENTED_EDGE('',*,*,#6130,.T.);
#8162=ORIENTED_EDGE('',*,*,#6050,.T.);
#8163=ORIENTED_EDGE('',*,*,#6053,.T.);
#8164=ORIENTED_EDGE('',*,*,#6131,.T.);
#8165=ORIENTED_EDGE('',*,*,#6132,.T.);
#8166=ORIENTED_EDGE('',*,*,#6130,.F.);
#8167=ORIENTED_EDGE('',*,*,#6110,.T.);
#8168=ORIENTED_EDGE('',*,*,#6131,.F.);
#8169=ORIENTED_EDGE('',*,*,#6109,.T.);
#8170=ORIENTED_EDGE('',*,*,#6133,.T.);
#8171=ORIENTED_EDGE('',*,*,#6119,.T.);
#8172=ORIENTED_EDGE('',*,*,#6134,.T.);
#8173=ORIENTED_EDGE('',*,*,#6135,.T.);
#8174=ORIENTED_EDGE('',*,*,#6134,.F.);
#8175=ORIENTED_EDGE('',*,*,#6136,.F.);
#8176=ORIENTED_EDGE('',*,*,#6137,.T.);
#8177=ORIENTED_EDGE('',*,*,#6135,.F.);
#8178=ORIENTED_EDGE('',*,*,#6137,.F.);
#8179=ORIENTED_EDGE('',*,*,#6081,.T.);
#8180=ORIENTED_EDGE('',*,*,#6138,.T.);
#8181=ORIENTED_EDGE('',*,*,#6136,.T.);
#8182=ORIENTED_EDGE('',*,*,#6138,.F.);
#8183=ORIENTED_EDGE('',*,*,#6116,.T.);
#8184=ORIENTED_EDGE('',*,*,#6139,.T.);
#8185=ORIENTED_EDGE('',*,*,#6140,.T.);
#8186=ORIENTED_EDGE('',*,*,#6139,.F.);
#8187=ORIENTED_EDGE('',*,*,#6141,.F.);
#8188=ORIENTED_EDGE('',*,*,#6142,.T.);
#8189=ORIENTED_EDGE('',*,*,#6140,.F.);
#8190=ORIENTED_EDGE('',*,*,#6142,.F.);
#8191=ORIENTED_EDGE('',*,*,#6078,.T.);
#8192=ORIENTED_EDGE('',*,*,#6143,.T.);
#8193=ORIENTED_EDGE('',*,*,#6141,.T.);
#8194=ORIENTED_EDGE('',*,*,#6143,.F.);
#8195=ORIENTED_EDGE('',*,*,#6118,.T.);
#8196=ORIENTED_EDGE('',*,*,#6144,.T.);
#8197=ORIENTED_EDGE('',*,*,#6145,.T.);
#8198=ORIENTED_EDGE('',*,*,#6144,.F.);
#8199=ORIENTED_EDGE('',*,*,#6146,.F.);
#8200=ORIENTED_EDGE('',*,*,#6147,.T.);
#8201=ORIENTED_EDGE('',*,*,#6145,.F.);
#8202=ORIENTED_EDGE('',*,*,#6147,.F.);
#8203=ORIENTED_EDGE('',*,*,#6080,.T.);
#8204=ORIENTED_EDGE('',*,*,#6148,.T.);
#8205=ORIENTED_EDGE('',*,*,#6146,.T.);
#8206=ORIENTED_EDGE('',*,*,#6148,.F.);
#8207=ORIENTED_EDGE('',*,*,#6117,.T.);
#8208=ORIENTED_EDGE('',*,*,#6149,.T.);
#8209=ORIENTED_EDGE('',*,*,#6150,.T.);
#8210=ORIENTED_EDGE('',*,*,#6149,.F.);
#8211=ORIENTED_EDGE('',*,*,#6151,.F.);
#8212=ORIENTED_EDGE('',*,*,#6152,.T.);
#8213=ORIENTED_EDGE('',*,*,#6150,.F.);
#8214=ORIENTED_EDGE('',*,*,#6152,.F.);
#8215=ORIENTED_EDGE('',*,*,#6079,.T.);
#8216=ORIENTED_EDGE('',*,*,#6153,.T.);
#8217=ORIENTED_EDGE('',*,*,#6151,.T.);
#8218=ORIENTED_EDGE('',*,*,#6153,.F.);
#8219=ORIENTED_EDGE('',*,*,#6154,.F.);
#8220=ORIENTED_EDGE('',*,*,#6155,.T.);
#8221=ORIENTED_EDGE('',*,*,#6156,.T.);
#8222=ORIENTED_EDGE('',*,*,#6155,.F.);
#8223=ORIENTED_EDGE('',*,*,#6156,.F.);
#8224=ORIENTED_EDGE('',*,*,#6157,.T.);
#8225=ORIENTED_EDGE('',*,*,#6158,.T.);
#8226=ORIENTED_EDGE('',*,*,#6157,.F.);
#8227=ORIENTED_EDGE('',*,*,#6158,.F.);
#8228=ORIENTED_EDGE('',*,*,#6159,.T.);
#8229=ORIENTED_EDGE('',*,*,#6159,.F.);
#8230=ORIENTED_EDGE('',*,*,#6160,.T.);
#8231=ORIENTED_EDGE('',*,*,#6161,.T.);
#8232=ORIENTED_EDGE('',*,*,#6160,.F.);
#8233=ORIENTED_EDGE('',*,*,#6162,.T.);
#8234=ORIENTED_EDGE('',*,*,#6161,.F.);
#8235=ORIENTED_EDGE('',*,*,#6162,.F.);
#8236=ORIENTED_EDGE('',*,*,#6163,.T.);
#8237=ORIENTED_EDGE('',*,*,#6164,.T.);
#8238=ORIENTED_EDGE('',*,*,#6163,.F.);
#8239=ORIENTED_EDGE('',*,*,#6164,.F.);
#8240=ORIENTED_EDGE('',*,*,#6165,.T.);
#8241=ORIENTED_EDGE('',*,*,#6166,.F.);
#8242=ORIENTED_EDGE('',*,*,#6165,.F.);
#8243=ORIENTED_EDGE('',*,*,#6048,.F.);
#8244=ORIENTED_EDGE('',*,*,#6167,.T.);
#8245=ORIENTED_EDGE('',*,*,#6168,.T.);
#8246=ORIENTED_EDGE('',*,*,#6167,.F.);
#8247=ORIENTED_EDGE('',*,*,#6168,.F.);
#8248=ORIENTED_EDGE('',*,*,#6169,.T.);
#8249=ORIENTED_EDGE('',*,*,#6170,.T.);
#8250=ORIENTED_EDGE('',*,*,#6169,.F.);
#8251=ORIENTED_EDGE('',*,*,#6170,.F.);
#8252=ORIENTED_EDGE('',*,*,#6171,.T.);
#8253=ORIENTED_EDGE('',*,*,#6171,.F.);
#8254=ORIENTED_EDGE('',*,*,#6172,.T.);
#8255=ORIENTED_EDGE('',*,*,#6173,.T.);
#8256=ORIENTED_EDGE('',*,*,#6172,.F.);
#8257=ORIENTED_EDGE('',*,*,#6174,.T.);
#8258=ORIENTED_EDGE('',*,*,#6173,.F.);
#8259=ORIENTED_EDGE('',*,*,#6174,.F.);
#8260=ORIENTED_EDGE('',*,*,#6175,.T.);
#8261=ORIENTED_EDGE('',*,*,#6176,.T.);
#8262=ORIENTED_EDGE('',*,*,#6175,.F.);
#8263=ORIENTED_EDGE('',*,*,#6176,.F.);
#8264=ORIENTED_EDGE('',*,*,#6177,.T.);
#8265=ORIENTED_EDGE('',*,*,#5989,.F.);
#8266=ORIENTED_EDGE('',*,*,#6177,.F.);
#8267=ORIENTED_EDGE('',*,*,#5943,.F.);
#8268=ORIENTED_EDGE('',*,*,#6178,.T.);
#8269=ORIENTED_EDGE('',*,*,#6179,.T.);
#8270=ORIENTED_EDGE('',*,*,#6178,.F.);
#8271=ORIENTED_EDGE('',*,*,#6179,.F.);
#8272=ORIENTED_EDGE('',*,*,#6180,.T.);
#8273=ORIENTED_EDGE('',*,*,#6181,.T.);
#8274=ORIENTED_EDGE('',*,*,#6180,.F.);
#8275=ORIENTED_EDGE('',*,*,#6181,.F.);
#8276=ORIENTED_EDGE('',*,*,#6182,.T.);
#8277=ORIENTED_EDGE('',*,*,#6182,.F.);
#8278=ORIENTED_EDGE('',*,*,#6183,.T.);
#8279=ORIENTED_EDGE('',*,*,#6184,.T.);
#8280=ORIENTED_EDGE('',*,*,#6183,.F.);
#8281=ORIENTED_EDGE('',*,*,#6185,.T.);
#8282=ORIENTED_EDGE('',*,*,#6184,.F.);
#8283=ORIENTED_EDGE('',*,*,#6185,.F.);
#8284=ORIENTED_EDGE('',*,*,#6186,.T.);
#8285=ORIENTED_EDGE('',*,*,#6187,.T.);
#8286=ORIENTED_EDGE('',*,*,#6186,.F.);
#8287=ORIENTED_EDGE('',*,*,#6187,.F.);
#8288=ORIENTED_EDGE('',*,*,#6188,.T.);
#8289=ORIENTED_EDGE('',*,*,#5899,.F.);
#8290=ORIENTED_EDGE('',*,*,#6188,.F.);
#8291=ORIENTED_EDGE('',*,*,#6189,.T.);
#8292=ORIENTED_EDGE('',*,*,#6066,.T.);
#8293=ORIENTED_EDGE('',*,*,#6084,.T.);
#8294=ORIENTED_EDGE('',*,*,#6190,.T.);
#8295=ORIENTED_EDGE('',*,*,#6191,.T.);
#8296=ORIENTED_EDGE('',*,*,#6104,.T.);
#8297=ORIENTED_EDGE('',*,*,#6122,.T.);
#8298=ORIENTED_EDGE('',*,*,#6192,.T.);
#8299=ORIENTED_EDGE('',*,*,#6028,.F.);
#8300=ORIENTED_EDGE('',*,*,#6054,.T.);
#8301=ORIENTED_EDGE('',*,*,#6038,.F.);
#8302=ORIENTED_EDGE('',*,*,#6033,.T.);
#8303=ORIENTED_EDGE('',*,*,#6003,.F.);
#8304=ORIENTED_EDGE('',*,*,#6026,.T.);
#8305=ORIENTED_EDGE('',*,*,#6011,.F.);
#8306=ORIENTED_EDGE('',*,*,#6006,.T.);
#8307=ORIENTED_EDGE('',*,*,#5925,.F.);
#8308=ORIENTED_EDGE('',*,*,#5950,.T.);
#8309=ORIENTED_EDGE('',*,*,#5935,.F.);
#8310=ORIENTED_EDGE('',*,*,#5930,.T.);
#8311=ORIENTED_EDGE('',*,*,#5889,.F.);
#8312=ORIENTED_EDGE('',*,*,#5923,.T.);
#8313=ORIENTED_EDGE('',*,*,#5908,.F.);
#8314=ORIENTED_EDGE('',*,*,#5903,.T.);
#8315=ORIENTED_EDGE('',*,*,#5893,.F.);
#8316=ORIENTED_EDGE('',*,*,#5898,.T.);
#8317=ORIENTED_EDGE('',*,*,#6120,.T.);
#8318=ORIENTED_EDGE('',*,*,#6096,.F.);
#8319=ORIENTED_EDGE('',*,*,#5920,.T.);
#8320=ORIENTED_EDGE('',*,*,#5975,.F.);
#8321=ORIENTED_EDGE('',*,*,#5998,.T.);
#8322=ORIENTED_EDGE('',*,*,#6129,.F.);
#8323=ORIENTED_EDGE('',*,*,#6023,.T.);
#8324=ORIENTED_EDGE('',*,*,#6005,.F.);
#8325=ORIENTED_EDGE('',*,*,#5987,.T.);
#8326=ORIENTED_EDGE('',*,*,#6042,.F.);
#8327=ORIENTED_EDGE('',*,*,#6047,.T.);
#8328=ORIENTED_EDGE('',*,*,#6082,.T.);
#8329=ORIENTED_EDGE('',*,*,#6058,.F.);
#8330=ORIENTED_EDGE('',*,*,#6035,.T.);
#8331=ORIENTED_EDGE('',*,*,#6193,.T.);
#8332=ORIENTED_EDGE('',*,*,#6194,.T.);
#8333=ORIENTED_EDGE('',*,*,#6195,.T.);
#8334=ORIENTED_EDGE('',*,*,#6070,.T.);
#8335=ORIENTED_EDGE('',*,*,#6092,.F.);
#8336=ORIENTED_EDGE('',*,*,#6195,.F.);
#8337=ORIENTED_EDGE('',*,*,#6196,.T.);
#8338=ORIENTED_EDGE('',*,*,#5902,.F.);
#8339=ORIENTED_EDGE('',*,*,#6091,.F.);
#8340=ORIENTED_EDGE('',*,*,#6197,.T.);
#8341=ORIENTED_EDGE('',*,*,#6198,.T.);
#8342=ORIENTED_EDGE('',*,*,#6199,.T.);
#8343=ORIENTED_EDGE('',*,*,#6108,.T.);
#8344=ORIENTED_EDGE('',*,*,#6133,.F.);
#8345=ORIENTED_EDGE('',*,*,#6199,.F.);
#8346=ORIENTED_EDGE('',*,*,#6200,.T.);
#8347=ORIENTED_EDGE('',*,*,#6051,.F.);
#8348=ORIENTED_EDGE('',*,*,#6132,.F.);
#8349=ORIENTED_EDGE('',*,*,#6189,.F.);
#8350=ORIENTED_EDGE('',*,*,#6201,.T.);
#8351=ORIENTED_EDGE('',*,*,#6067,.T.);
#8352=ORIENTED_EDGE('',*,*,#6191,.F.);
#8353=ORIENTED_EDGE('',*,*,#6202,.T.);
#8354=ORIENTED_EDGE('',*,*,#6105,.T.);
#8355=ORIENTED_EDGE('',*,*,#6193,.F.);
#8356=ORIENTED_EDGE('',*,*,#6069,.T.);
#8357=ORIENTED_EDGE('',*,*,#6203,.T.);
#8358=ORIENTED_EDGE('',*,*,#6197,.F.);
#8359=ORIENTED_EDGE('',*,*,#6107,.T.);
#8360=ORIENTED_EDGE('',*,*,#6204,.T.);
#8361=ORIENTED_EDGE('',*,*,#6201,.F.);
#8362=ORIENTED_EDGE('',*,*,#6190,.F.);
#8363=ORIENTED_EDGE('',*,*,#6083,.F.);
#8364=ORIENTED_EDGE('',*,*,#6046,.T.);
#8365=ORIENTED_EDGE('',*,*,#6205,.T.);
#8366=ORIENTED_EDGE('',*,*,#6206,.T.);
#8367=ORIENTED_EDGE('',*,*,#6200,.F.);
#8368=ORIENTED_EDGE('',*,*,#6198,.F.);
#8369=ORIENTED_EDGE('',*,*,#6204,.F.);
#8370=ORIENTED_EDGE('',*,*,#6207,.T.);
#8371=ORIENTED_EDGE('',*,*,#6208,.F.);
#8372=ORIENTED_EDGE('',*,*,#6044,.T.);
#8373=ORIENTED_EDGE('',*,*,#5966,.F.);
#8374=ORIENTED_EDGE('',*,*,#6001,.F.);
#8375=ORIENTED_EDGE('',*,*,#5992,.F.);
#8376=ORIENTED_EDGE('',*,*,#5968,.F.);
#8377=ORIENTED_EDGE('',*,*,#6166,.T.);
#8378=ORIENTED_EDGE('',*,*,#6121,.F.);
#8379=ORIENTED_EDGE('',*,*,#5897,.T.);
#8380=ORIENTED_EDGE('',*,*,#6209,.T.);
#8381=ORIENTED_EDGE('',*,*,#6210,.T.);
#8382=ORIENTED_EDGE('',*,*,#6202,.F.);
#8383=ORIENTED_EDGE('',*,*,#6192,.F.);
#8384=ORIENTED_EDGE('',*,*,#6211,.T.);
#8385=ORIENTED_EDGE('',*,*,#6212,.T.);
#8386=ORIENTED_EDGE('',*,*,#6209,.F.);
#8387=ORIENTED_EDGE('',*,*,#5896,.T.);
#8388=ORIENTED_EDGE('',*,*,#6203,.F.);
#8389=ORIENTED_EDGE('',*,*,#6213,.T.);
#8390=ORIENTED_EDGE('',*,*,#6211,.F.);
#8391=ORIENTED_EDGE('',*,*,#5895,.T.);
#8392=ORIENTED_EDGE('',*,*,#6196,.F.);
#8393=ORIENTED_EDGE('',*,*,#6194,.F.);
#8394=ORIENTED_EDGE('',*,*,#6208,.T.);
#8395=ORIENTED_EDGE('',*,*,#6214,.T.);
#8396=ORIENTED_EDGE('',*,*,#6205,.F.);
#8397=ORIENTED_EDGE('',*,*,#6045,.T.);
#8398=ORIENTED_EDGE('',*,*,#6210,.F.);
#8399=ORIENTED_EDGE('',*,*,#6215,.T.);
#8400=ORIENTED_EDGE('',*,*,#6207,.F.);
#8401=ORIENTED_EDGE('',*,*,#6106,.T.);
#8402=ORIENTED_EDGE('',*,*,#6212,.F.);
#8403=ORIENTED_EDGE('',*,*,#6216,.F.);
#8404=ORIENTED_EDGE('',*,*,#6214,.F.);
#8405=ORIENTED_EDGE('',*,*,#6215,.F.);
#8406=ORIENTED_EDGE('',*,*,#6154,.T.);
#8407=ORIENTED_EDGE('',*,*,#6213,.F.);
#8408=ORIENTED_EDGE('',*,*,#6068,.T.);
#8409=ORIENTED_EDGE('',*,*,#6206,.F.);
#8410=ORIENTED_EDGE('',*,*,#6216,.T.);
#8411=ORIENTED_EDGE('',*,*,#6217,.T.);
#8412=ORIENTED_EDGE('',*,*,#6218,.T.);
#8413=ORIENTED_EDGE('',*,*,#6219,.T.);
#8414=ORIENTED_EDGE('',*,*,#6220,.T.);
#8415=ORIENTED_EDGE('',*,*,#6218,.F.);
#8416=ORIENTED_EDGE('',*,*,#6219,.F.);
#8417=ORIENTED_EDGE('',*,*,#6220,.F.);
#8418=ORIENTED_EDGE('',*,*,#6221,.T.);
#8419=ORIENTED_EDGE('',*,*,#6222,.T.);
#8420=ORIENTED_EDGE('',*,*,#6223,.T.);
#8421=ORIENTED_EDGE('',*,*,#6224,.T.);
#8422=ORIENTED_EDGE('',*,*,#6225,.T.);
#8423=ORIENTED_EDGE('',*,*,#6226,.T.);
#8424=ORIENTED_EDGE('',*,*,#6227,.T.);
#8425=ORIENTED_EDGE('',*,*,#6228,.T.);
#8426=ORIENTED_EDGE('',*,*,#6229,.T.);
#8427=ORIENTED_EDGE('',*,*,#6230,.T.);
#8428=ORIENTED_EDGE('',*,*,#6231,.T.);
#8429=ORIENTED_EDGE('',*,*,#6232,.T.);
#8430=ORIENTED_EDGE('',*,*,#6233,.T.);
#8431=ORIENTED_EDGE('',*,*,#6234,.T.);
#8432=ORIENTED_EDGE('',*,*,#6235,.T.);
#8433=ORIENTED_EDGE('',*,*,#6236,.T.);
#8434=ORIENTED_EDGE('',*,*,#6237,.T.);
#8435=ORIENTED_EDGE('',*,*,#6238,.T.);
#8436=ORIENTED_EDGE('',*,*,#6239,.T.);
#8437=ORIENTED_EDGE('',*,*,#6240,.T.);
#8438=ORIENTED_EDGE('',*,*,#6241,.T.);
#8439=ORIENTED_EDGE('',*,*,#6242,.T.);
#8440=ORIENTED_EDGE('',*,*,#6243,.T.);
#8441=ORIENTED_EDGE('',*,*,#6244,.T.);
#8442=ORIENTED_EDGE('',*,*,#6245,.T.);
#8443=ORIENTED_EDGE('',*,*,#6246,.T.);
#8444=ORIENTED_EDGE('',*,*,#6247,.T.);
#8445=ORIENTED_EDGE('',*,*,#6248,.T.);
#8446=ORIENTED_EDGE('',*,*,#6249,.T.);
#8447=ORIENTED_EDGE('',*,*,#6250,.T.);
#8448=ORIENTED_EDGE('',*,*,#6251,.T.);
#8449=ORIENTED_EDGE('',*,*,#6252,.T.);
#8450=ORIENTED_EDGE('',*,*,#6253,.T.);
#8451=ORIENTED_EDGE('',*,*,#6254,.T.);
#8452=ORIENTED_EDGE('',*,*,#6255,.T.);
#8453=ORIENTED_EDGE('',*,*,#6256,.T.);
#8454=ORIENTED_EDGE('',*,*,#6257,.T.);
#8455=ORIENTED_EDGE('',*,*,#6258,.T.);
#8456=ORIENTED_EDGE('',*,*,#6259,.T.);
#8457=ORIENTED_EDGE('',*,*,#6260,.T.);
#8458=ORIENTED_EDGE('',*,*,#6261,.T.);
#8459=ORIENTED_EDGE('',*,*,#6262,.T.);
#8460=ORIENTED_EDGE('',*,*,#6263,.T.);
#8461=ORIENTED_EDGE('',*,*,#6264,.T.);
#8462=ORIENTED_EDGE('',*,*,#6265,.T.);
#8463=ORIENTED_EDGE('',*,*,#6266,.T.);
#8464=ORIENTED_EDGE('',*,*,#6267,.T.);
#8465=ORIENTED_EDGE('',*,*,#6268,.T.);
#8466=ORIENTED_EDGE('',*,*,#6269,.T.);
#8467=ORIENTED_EDGE('',*,*,#6270,.T.);
#8468=ORIENTED_EDGE('',*,*,#6271,.T.);
#8469=ORIENTED_EDGE('',*,*,#6272,.T.);
#8470=ORIENTED_EDGE('',*,*,#6273,.T.);
#8471=ORIENTED_EDGE('',*,*,#6274,.T.);
#8472=ORIENTED_EDGE('',*,*,#6275,.T.);
#8473=ORIENTED_EDGE('',*,*,#6276,.T.);
#8474=ORIENTED_EDGE('',*,*,#6277,.T.);
#8475=ORIENTED_EDGE('',*,*,#6278,.T.);
#8476=ORIENTED_EDGE('',*,*,#6279,.T.);
#8477=ORIENTED_EDGE('',*,*,#6280,.T.);
#8478=ORIENTED_EDGE('',*,*,#6281,.T.);
#8479=ORIENTED_EDGE('',*,*,#6282,.T.);
#8480=ORIENTED_EDGE('',*,*,#6283,.T.);
#8481=ORIENTED_EDGE('',*,*,#6284,.T.);
#8482=ORIENTED_EDGE('',*,*,#6285,.T.);
#8483=ORIENTED_EDGE('',*,*,#6286,.T.);
#8484=ORIENTED_EDGE('',*,*,#6287,.T.);
#8485=ORIENTED_EDGE('',*,*,#6288,.T.);
#8486=ORIENTED_EDGE('',*,*,#6289,.T.);
#8487=ORIENTED_EDGE('',*,*,#6290,.T.);
#8488=ORIENTED_EDGE('',*,*,#6291,.T.);
#8489=ORIENTED_EDGE('',*,*,#6292,.T.);
#8490=ORIENTED_EDGE('',*,*,#6293,.T.);
#8491=ORIENTED_EDGE('',*,*,#6294,.T.);
#8492=ORIENTED_EDGE('',*,*,#6295,.T.);
#8493=ORIENTED_EDGE('',*,*,#6296,.T.);
#8494=ORIENTED_EDGE('',*,*,#6297,.T.);
#8495=ORIENTED_EDGE('',*,*,#6298,.T.);
#8496=ORIENTED_EDGE('',*,*,#6299,.T.);
#8497=ORIENTED_EDGE('',*,*,#6300,.T.);
#8498=ORIENTED_EDGE('',*,*,#6301,.T.);
#8499=ORIENTED_EDGE('',*,*,#6302,.T.);
#8500=ORIENTED_EDGE('',*,*,#6221,.F.);
#8501=ORIENTED_EDGE('',*,*,#6217,.F.);
#8502=ORIENTED_EDGE('',*,*,#6303,.F.);
#8503=ORIENTED_EDGE('',*,*,#6304,.T.);
#8504=ORIENTED_EDGE('',*,*,#6305,.F.);
#8505=ORIENTED_EDGE('',*,*,#6306,.T.);
#8506=ORIENTED_EDGE('',*,*,#6306,.F.);
#8507=ORIENTED_EDGE('',*,*,#6307,.T.);
#8508=ORIENTED_EDGE('',*,*,#6308,.T.);
#8509=ORIENTED_EDGE('',*,*,#6309,.T.);
#8510=ORIENTED_EDGE('',*,*,#6310,.T.);
#8511=ORIENTED_EDGE('',*,*,#6311,.T.);
#8512=ORIENTED_EDGE('',*,*,#6309,.F.);
#8513=ORIENTED_EDGE('',*,*,#6312,.T.);
#8514=ORIENTED_EDGE('',*,*,#6313,.T.);
#8515=ORIENTED_EDGE('',*,*,#6313,.F.);
#8516=ORIENTED_EDGE('',*,*,#6314,.F.);
#8517=ORIENTED_EDGE('',*,*,#6315,.F.);
#8518=ORIENTED_EDGE('',*,*,#6316,.F.);
#8519=ORIENTED_EDGE('',*,*,#6303,.T.);
#8520=ORIENTED_EDGE('',*,*,#6307,.F.);
#8521=ORIENTED_EDGE('',*,*,#6305,.T.);
#8522=ORIENTED_EDGE('',*,*,#6317,.F.);
#8523=ORIENTED_EDGE('',*,*,#6318,.F.);
#8524=ORIENTED_EDGE('',*,*,#6310,.F.);
#8525=ORIENTED_EDGE('',*,*,#6311,.F.);
#8526=ORIENTED_EDGE('',*,*,#6319,.T.);
#8527=ORIENTED_EDGE('',*,*,#6320,.F.);
#8528=ORIENTED_EDGE('',*,*,#6321,.F.);
#8529=ORIENTED_EDGE('',*,*,#6319,.F.);
#8530=ORIENTED_EDGE('',*,*,#6304,.F.);
#8531=ORIENTED_EDGE('',*,*,#6316,.T.);
#8532=ORIENTED_EDGE('',*,*,#6322,.T.);
#8533=ORIENTED_EDGE('',*,*,#6323,.T.);
#8534=ORIENTED_EDGE('',*,*,#6324,.T.);
#8535=ORIENTED_EDGE('',*,*,#6325,.T.);
#8536=ORIENTED_EDGE('',*,*,#6323,.F.);
#8537=ORIENTED_EDGE('',*,*,#6326,.T.);
#8538=ORIENTED_EDGE('',*,*,#6317,.T.);
#8539=ORIENTED_EDGE('',*,*,#6327,.F.);
#8540=ORIENTED_EDGE('',*,*,#6328,.F.);
#8541=ORIENTED_EDGE('',*,*,#6329,.T.);
#8542=ORIENTED_EDGE('',*,*,#6324,.F.);
#8543=ORIENTED_EDGE('',*,*,#6325,.F.);
#8544=ORIENTED_EDGE('',*,*,#6329,.F.);
#8545=ORIENTED_EDGE('',*,*,#6330,.F.);
#8546=ORIENTED_EDGE('',*,*,#6331,.T.);
#8547=ORIENTED_EDGE('',*,*,#6314,.T.);
#8548=ORIENTED_EDGE('',*,*,#6312,.F.);
#8549=ORIENTED_EDGE('',*,*,#6308,.F.);
#8550=ORIENTED_EDGE('',*,*,#6318,.T.);
#8551=ORIENTED_EDGE('',*,*,#6326,.F.);
#8552=ORIENTED_EDGE('',*,*,#6322,.F.);
#8553=ORIENTED_EDGE('',*,*,#6315,.T.);
#8554=ORIENTED_EDGE('',*,*,#6331,.F.);
#8555=ORIENTED_EDGE('',*,*,#6332,.F.);
#8556=ORIENTED_EDGE('',*,*,#6333,.T.);
#8557=ORIENTED_EDGE('',*,*,#6254,.F.);
#8558=ORIENTED_EDGE('',*,*,#6334,.F.);
#8559=ORIENTED_EDGE('',*,*,#6335,.F.);
#8560=ORIENTED_EDGE('',*,*,#6336,.F.);
#8561=ORIENTED_EDGE('',*,*,#6256,.F.);
#8562=ORIENTED_EDGE('',*,*,#6337,.F.);
#8563=ORIENTED_EDGE('',*,*,#6338,.F.);
#8564=ORIENTED_EDGE('',*,*,#6337,.T.);
#8565=ORIENTED_EDGE('',*,*,#6255,.F.);
#8566=ORIENTED_EDGE('',*,*,#6333,.F.);
#8567=ORIENTED_EDGE('',*,*,#6336,.T.);
#8568=ORIENTED_EDGE('',*,*,#6339,.T.);
#8569=ORIENTED_EDGE('',*,*,#6340,.T.);
#8570=ORIENTED_EDGE('',*,*,#6257,.F.);
#8571=ORIENTED_EDGE('',*,*,#6334,.T.);
#8572=ORIENTED_EDGE('',*,*,#6253,.F.);
#8573=ORIENTED_EDGE('',*,*,#6341,.T.);
#8574=ORIENTED_EDGE('',*,*,#6342,.T.);
#8575=ORIENTED_EDGE('',*,*,#6343,.F.);
#8576=ORIENTED_EDGE('',*,*,#6344,.T.);
#8577=ORIENTED_EDGE('',*,*,#6250,.F.);
#8578=ORIENTED_EDGE('',*,*,#6345,.F.);
#8579=ORIENTED_EDGE('',*,*,#6346,.F.);
#8580=ORIENTED_EDGE('',*,*,#6341,.F.);
#8581=ORIENTED_EDGE('',*,*,#6252,.F.);
#8582=ORIENTED_EDGE('',*,*,#6347,.F.);
#8583=ORIENTED_EDGE('',*,*,#6348,.F.);
#8584=ORIENTED_EDGE('',*,*,#6347,.T.);
#8585=ORIENTED_EDGE('',*,*,#6251,.F.);
#8586=ORIENTED_EDGE('',*,*,#6344,.F.);
#8587=ORIENTED_EDGE('',*,*,#6345,.T.);
#8588=ORIENTED_EDGE('',*,*,#6249,.F.);
#8589=ORIENTED_EDGE('',*,*,#6349,.T.);
#8590=ORIENTED_EDGE('',*,*,#6350,.T.);
#8591=ORIENTED_EDGE('',*,*,#6351,.F.);
#8592=ORIENTED_EDGE('',*,*,#6352,.T.);
#8593=ORIENTED_EDGE('',*,*,#6246,.F.);
#8594=ORIENTED_EDGE('',*,*,#6353,.F.);
#8595=ORIENTED_EDGE('',*,*,#6354,.F.);
#8596=ORIENTED_EDGE('',*,*,#6349,.F.);
#8597=ORIENTED_EDGE('',*,*,#6248,.F.);
#8598=ORIENTED_EDGE('',*,*,#6355,.F.);
#8599=ORIENTED_EDGE('',*,*,#6356,.F.);
#8600=ORIENTED_EDGE('',*,*,#6355,.T.);
#8601=ORIENTED_EDGE('',*,*,#6247,.F.);
#8602=ORIENTED_EDGE('',*,*,#6352,.F.);
#8603=ORIENTED_EDGE('',*,*,#6353,.T.);
#8604=ORIENTED_EDGE('',*,*,#6245,.F.);
#8605=ORIENTED_EDGE('',*,*,#6357,.T.);
#8606=ORIENTED_EDGE('',*,*,#6358,.T.);
#8607=ORIENTED_EDGE('',*,*,#6359,.F.);
#8608=ORIENTED_EDGE('',*,*,#6360,.T.);
#8609=ORIENTED_EDGE('',*,*,#6242,.F.);
#8610=ORIENTED_EDGE('',*,*,#6361,.F.);
#8611=ORIENTED_EDGE('',*,*,#6362,.F.);
#8612=ORIENTED_EDGE('',*,*,#6357,.F.);
#8613=ORIENTED_EDGE('',*,*,#6244,.F.);
#8614=ORIENTED_EDGE('',*,*,#6363,.F.);
#8615=ORIENTED_EDGE('',*,*,#6364,.F.);
#8616=ORIENTED_EDGE('',*,*,#6363,.T.);
#8617=ORIENTED_EDGE('',*,*,#6243,.F.);
#8618=ORIENTED_EDGE('',*,*,#6360,.F.);
#8619=ORIENTED_EDGE('',*,*,#6361,.T.);
#8620=ORIENTED_EDGE('',*,*,#6241,.F.);
#8621=ORIENTED_EDGE('',*,*,#6365,.T.);
#8622=ORIENTED_EDGE('',*,*,#6366,.T.);
#8623=ORIENTED_EDGE('',*,*,#6367,.F.);
#8624=ORIENTED_EDGE('',*,*,#6368,.T.);
#8625=ORIENTED_EDGE('',*,*,#6238,.F.);
#8626=ORIENTED_EDGE('',*,*,#6369,.F.);
#8627=ORIENTED_EDGE('',*,*,#6370,.F.);
#8628=ORIENTED_EDGE('',*,*,#6365,.F.);
#8629=ORIENTED_EDGE('',*,*,#6240,.F.);
#8630=ORIENTED_EDGE('',*,*,#6371,.F.);
#8631=ORIENTED_EDGE('',*,*,#6372,.F.);
#8632=ORIENTED_EDGE('',*,*,#6371,.T.);
#8633=ORIENTED_EDGE('',*,*,#6239,.F.);
#8634=ORIENTED_EDGE('',*,*,#6368,.F.);
#8635=ORIENTED_EDGE('',*,*,#6369,.T.);
#8636=ORIENTED_EDGE('',*,*,#6237,.F.);
#8637=ORIENTED_EDGE('',*,*,#6373,.T.);
#8638=ORIENTED_EDGE('',*,*,#6374,.T.);
#8639=ORIENTED_EDGE('',*,*,#6375,.F.);
#8640=ORIENTED_EDGE('',*,*,#6376,.T.);
#8641=ORIENTED_EDGE('',*,*,#6234,.F.);
#8642=ORIENTED_EDGE('',*,*,#6377,.F.);
#8643=ORIENTED_EDGE('',*,*,#6378,.F.);
#8644=ORIENTED_EDGE('',*,*,#6373,.F.);
#8645=ORIENTED_EDGE('',*,*,#6236,.F.);
#8646=ORIENTED_EDGE('',*,*,#6379,.F.);
#8647=ORIENTED_EDGE('',*,*,#6380,.F.);
#8648=ORIENTED_EDGE('',*,*,#6379,.T.);
#8649=ORIENTED_EDGE('',*,*,#6235,.F.);
#8650=ORIENTED_EDGE('',*,*,#6376,.F.);
#8651=ORIENTED_EDGE('',*,*,#6377,.T.);
#8652=ORIENTED_EDGE('',*,*,#6233,.F.);
#8653=ORIENTED_EDGE('',*,*,#6381,.T.);
#8654=ORIENTED_EDGE('',*,*,#6382,.T.);
#8655=ORIENTED_EDGE('',*,*,#6383,.F.);
#8656=ORIENTED_EDGE('',*,*,#6384,.T.);
#8657=ORIENTED_EDGE('',*,*,#6230,.F.);
#8658=ORIENTED_EDGE('',*,*,#6385,.F.);
#8659=ORIENTED_EDGE('',*,*,#6386,.F.);
#8660=ORIENTED_EDGE('',*,*,#6381,.F.);
#8661=ORIENTED_EDGE('',*,*,#6232,.F.);
#8662=ORIENTED_EDGE('',*,*,#6387,.F.);
#8663=ORIENTED_EDGE('',*,*,#6388,.F.);
#8664=ORIENTED_EDGE('',*,*,#6387,.T.);
#8665=ORIENTED_EDGE('',*,*,#6231,.F.);
#8666=ORIENTED_EDGE('',*,*,#6384,.F.);
#8667=ORIENTED_EDGE('',*,*,#6385,.T.);
#8668=ORIENTED_EDGE('',*,*,#6229,.F.);
#8669=ORIENTED_EDGE('',*,*,#6389,.T.);
#8670=ORIENTED_EDGE('',*,*,#6390,.T.);
#8671=ORIENTED_EDGE('',*,*,#6391,.F.);
#8672=ORIENTED_EDGE('',*,*,#6392,.T.);
#8673=ORIENTED_EDGE('',*,*,#6226,.F.);
#8674=ORIENTED_EDGE('',*,*,#6393,.F.);
#8675=ORIENTED_EDGE('',*,*,#6394,.F.);
#8676=ORIENTED_EDGE('',*,*,#6389,.F.);
#8677=ORIENTED_EDGE('',*,*,#6228,.F.);
#8678=ORIENTED_EDGE('',*,*,#6395,.F.);
#8679=ORIENTED_EDGE('',*,*,#6396,.F.);
#8680=ORIENTED_EDGE('',*,*,#6395,.T.);
#8681=ORIENTED_EDGE('',*,*,#6227,.F.);
#8682=ORIENTED_EDGE('',*,*,#6392,.F.);
#8683=ORIENTED_EDGE('',*,*,#6393,.T.);
#8684=ORIENTED_EDGE('',*,*,#6225,.F.);
#8685=ORIENTED_EDGE('',*,*,#6397,.T.);
#8686=ORIENTED_EDGE('',*,*,#6398,.T.);
#8687=ORIENTED_EDGE('',*,*,#6399,.F.);
#8688=ORIENTED_EDGE('',*,*,#6400,.T.);
#8689=ORIENTED_EDGE('',*,*,#6222,.F.);
#8690=ORIENTED_EDGE('',*,*,#6302,.F.);
#8691=ORIENTED_EDGE('',*,*,#6401,.F.);
#8692=ORIENTED_EDGE('',*,*,#6402,.F.);
#8693=ORIENTED_EDGE('',*,*,#6397,.F.);
#8694=ORIENTED_EDGE('',*,*,#6224,.F.);
#8695=ORIENTED_EDGE('',*,*,#6403,.F.);
#8696=ORIENTED_EDGE('',*,*,#6404,.F.);
#8697=ORIENTED_EDGE('',*,*,#6403,.T.);
#8698=ORIENTED_EDGE('',*,*,#6223,.F.);
#8699=ORIENTED_EDGE('',*,*,#6400,.F.);
#8700=ORIENTED_EDGE('',*,*,#6401,.T.);
#8701=ORIENTED_EDGE('',*,*,#6301,.F.);
#8702=ORIENTED_EDGE('',*,*,#6405,.T.);
#8703=ORIENTED_EDGE('',*,*,#6406,.T.);
#8704=ORIENTED_EDGE('',*,*,#6407,.F.);
#8705=ORIENTED_EDGE('',*,*,#6408,.T.);
#8706=ORIENTED_EDGE('',*,*,#6298,.F.);
#8707=ORIENTED_EDGE('',*,*,#6409,.F.);
#8708=ORIENTED_EDGE('',*,*,#6410,.F.);
#8709=ORIENTED_EDGE('',*,*,#6411,.F.);
#8710=ORIENTED_EDGE('',*,*,#6405,.F.);
#8711=ORIENTED_EDGE('',*,*,#6300,.F.);
#8712=ORIENTED_EDGE('',*,*,#6412,.F.);
#8713=ORIENTED_EDGE('',*,*,#6413,.F.);
#8714=ORIENTED_EDGE('',*,*,#6412,.T.);
#8715=ORIENTED_EDGE('',*,*,#6299,.F.);
#8716=ORIENTED_EDGE('',*,*,#6408,.F.);
#8717=ORIENTED_EDGE('',*,*,#6409,.T.);
#8718=ORIENTED_EDGE('',*,*,#6297,.F.);
#8719=ORIENTED_EDGE('',*,*,#6414,.T.);
#8720=ORIENTED_EDGE('',*,*,#6415,.T.);
#8721=ORIENTED_EDGE('',*,*,#6416,.F.);
#8722=ORIENTED_EDGE('',*,*,#6417,.T.);
#8723=ORIENTED_EDGE('',*,*,#6294,.F.);
#8724=ORIENTED_EDGE('',*,*,#6418,.F.);
#8725=ORIENTED_EDGE('',*,*,#6419,.F.);
#8726=ORIENTED_EDGE('',*,*,#6414,.F.);
#8727=ORIENTED_EDGE('',*,*,#6296,.F.);
#8728=ORIENTED_EDGE('',*,*,#6420,.F.);
#8729=ORIENTED_EDGE('',*,*,#6421,.F.);
#8730=ORIENTED_EDGE('',*,*,#6420,.T.);
#8731=ORIENTED_EDGE('',*,*,#6295,.F.);
#8732=ORIENTED_EDGE('',*,*,#6417,.F.);
#8733=ORIENTED_EDGE('',*,*,#6418,.T.);
#8734=ORIENTED_EDGE('',*,*,#6293,.F.);
#8735=ORIENTED_EDGE('',*,*,#6422,.T.);
#8736=ORIENTED_EDGE('',*,*,#6423,.T.);
#8737=ORIENTED_EDGE('',*,*,#6424,.F.);
#8738=ORIENTED_EDGE('',*,*,#6425,.T.);
#8739=ORIENTED_EDGE('',*,*,#6290,.F.);
#8740=ORIENTED_EDGE('',*,*,#6426,.F.);
#8741=ORIENTED_EDGE('',*,*,#6427,.F.);
#8742=ORIENTED_EDGE('',*,*,#6422,.F.);
#8743=ORIENTED_EDGE('',*,*,#6292,.F.);
#8744=ORIENTED_EDGE('',*,*,#6428,.F.);
#8745=ORIENTED_EDGE('',*,*,#6429,.F.);
#8746=ORIENTED_EDGE('',*,*,#6428,.T.);
#8747=ORIENTED_EDGE('',*,*,#6291,.F.);
#8748=ORIENTED_EDGE('',*,*,#6425,.F.);
#8749=ORIENTED_EDGE('',*,*,#6426,.T.);
#8750=ORIENTED_EDGE('',*,*,#6289,.F.);
#8751=ORIENTED_EDGE('',*,*,#6430,.T.);
#8752=ORIENTED_EDGE('',*,*,#6431,.T.);
#8753=ORIENTED_EDGE('',*,*,#6432,.F.);
#8754=ORIENTED_EDGE('',*,*,#6433,.T.);
#8755=ORIENTED_EDGE('',*,*,#6286,.F.);
#8756=ORIENTED_EDGE('',*,*,#6434,.F.);
#8757=ORIENTED_EDGE('',*,*,#6435,.F.);
#8758=ORIENTED_EDGE('',*,*,#6430,.F.);
#8759=ORIENTED_EDGE('',*,*,#6288,.F.);
#8760=ORIENTED_EDGE('',*,*,#6436,.F.);
#8761=ORIENTED_EDGE('',*,*,#6437,.F.);
#8762=ORIENTED_EDGE('',*,*,#6436,.T.);
#8763=ORIENTED_EDGE('',*,*,#6287,.F.);
#8764=ORIENTED_EDGE('',*,*,#6433,.F.);
#8765=ORIENTED_EDGE('',*,*,#6434,.T.);
#8766=ORIENTED_EDGE('',*,*,#6285,.F.);
#8767=ORIENTED_EDGE('',*,*,#6438,.T.);
#8768=ORIENTED_EDGE('',*,*,#6439,.T.);
#8769=ORIENTED_EDGE('',*,*,#6440,.F.);
#8770=ORIENTED_EDGE('',*,*,#6441,.T.);
#8771=ORIENTED_EDGE('',*,*,#6282,.F.);
#8772=ORIENTED_EDGE('',*,*,#6442,.F.);
#8773=ORIENTED_EDGE('',*,*,#6443,.F.);
#8774=ORIENTED_EDGE('',*,*,#6438,.F.);
#8775=ORIENTED_EDGE('',*,*,#6284,.F.);
#8776=ORIENTED_EDGE('',*,*,#6444,.F.);
#8777=ORIENTED_EDGE('',*,*,#6445,.F.);
#8778=ORIENTED_EDGE('',*,*,#6444,.T.);
#8779=ORIENTED_EDGE('',*,*,#6283,.F.);
#8780=ORIENTED_EDGE('',*,*,#6441,.F.);
#8781=ORIENTED_EDGE('',*,*,#6442,.T.);
#8782=ORIENTED_EDGE('',*,*,#6281,.F.);
#8783=ORIENTED_EDGE('',*,*,#6446,.T.);
#8784=ORIENTED_EDGE('',*,*,#6447,.T.);
#8785=ORIENTED_EDGE('',*,*,#6448,.F.);
#8786=ORIENTED_EDGE('',*,*,#6449,.T.);
#8787=ORIENTED_EDGE('',*,*,#6278,.F.);
#8788=ORIENTED_EDGE('',*,*,#6450,.F.);
#8789=ORIENTED_EDGE('',*,*,#6451,.F.);
#8790=ORIENTED_EDGE('',*,*,#6446,.F.);
#8791=ORIENTED_EDGE('',*,*,#6280,.F.);
#8792=ORIENTED_EDGE('',*,*,#6452,.F.);
#8793=ORIENTED_EDGE('',*,*,#6453,.F.);
#8794=ORIENTED_EDGE('',*,*,#6452,.T.);
#8795=ORIENTED_EDGE('',*,*,#6279,.F.);
#8796=ORIENTED_EDGE('',*,*,#6449,.F.);
#8797=ORIENTED_EDGE('',*,*,#6450,.T.);
#8798=ORIENTED_EDGE('',*,*,#6277,.F.);
#8799=ORIENTED_EDGE('',*,*,#6454,.T.);
#8800=ORIENTED_EDGE('',*,*,#6455,.T.);
#8801=ORIENTED_EDGE('',*,*,#6456,.F.);
#8802=ORIENTED_EDGE('',*,*,#6457,.T.);
#8803=ORIENTED_EDGE('',*,*,#6274,.F.);
#8804=ORIENTED_EDGE('',*,*,#6458,.F.);
#8805=ORIENTED_EDGE('',*,*,#6459,.F.);
#8806=ORIENTED_EDGE('',*,*,#6454,.F.);
#8807=ORIENTED_EDGE('',*,*,#6276,.F.);
#8808=ORIENTED_EDGE('',*,*,#6460,.F.);
#8809=ORIENTED_EDGE('',*,*,#6461,.F.);
#8810=ORIENTED_EDGE('',*,*,#6460,.T.);
#8811=ORIENTED_EDGE('',*,*,#6275,.F.);
#8812=ORIENTED_EDGE('',*,*,#6457,.F.);
#8813=ORIENTED_EDGE('',*,*,#6458,.T.);
#8814=ORIENTED_EDGE('',*,*,#6273,.F.);
#8815=ORIENTED_EDGE('',*,*,#6462,.T.);
#8816=ORIENTED_EDGE('',*,*,#6463,.T.);
#8817=ORIENTED_EDGE('',*,*,#6464,.F.);
#8818=ORIENTED_EDGE('',*,*,#6465,.T.);
#8819=ORIENTED_EDGE('',*,*,#6270,.F.);
#8820=ORIENTED_EDGE('',*,*,#6466,.F.);
#8821=ORIENTED_EDGE('',*,*,#6467,.F.);
#8822=ORIENTED_EDGE('',*,*,#6462,.F.);
#8823=ORIENTED_EDGE('',*,*,#6272,.F.);
#8824=ORIENTED_EDGE('',*,*,#6468,.F.);
#8825=ORIENTED_EDGE('',*,*,#6469,.F.);
#8826=ORIENTED_EDGE('',*,*,#6468,.T.);
#8827=ORIENTED_EDGE('',*,*,#6271,.F.);
#8828=ORIENTED_EDGE('',*,*,#6465,.F.);
#8829=ORIENTED_EDGE('',*,*,#6466,.T.);
#8830=ORIENTED_EDGE('',*,*,#6269,.F.);
#8831=ORIENTED_EDGE('',*,*,#6470,.T.);
#8832=ORIENTED_EDGE('',*,*,#6471,.T.);
#8833=ORIENTED_EDGE('',*,*,#6472,.F.);
#8834=ORIENTED_EDGE('',*,*,#6473,.T.);
#8835=ORIENTED_EDGE('',*,*,#6266,.F.);
#8836=ORIENTED_EDGE('',*,*,#6474,.F.);
#8837=ORIENTED_EDGE('',*,*,#6475,.F.);
#8838=ORIENTED_EDGE('',*,*,#6470,.F.);
#8839=ORIENTED_EDGE('',*,*,#6268,.F.);
#8840=ORIENTED_EDGE('',*,*,#6476,.F.);
#8841=ORIENTED_EDGE('',*,*,#6477,.F.);
#8842=ORIENTED_EDGE('',*,*,#6476,.T.);
#8843=ORIENTED_EDGE('',*,*,#6267,.F.);
#8844=ORIENTED_EDGE('',*,*,#6473,.F.);
#8845=ORIENTED_EDGE('',*,*,#6474,.T.);
#8846=ORIENTED_EDGE('',*,*,#6265,.F.);
#8847=ORIENTED_EDGE('',*,*,#6478,.T.);
#8848=ORIENTED_EDGE('',*,*,#6479,.T.);
#8849=ORIENTED_EDGE('',*,*,#6264,.F.);
#8850=ORIENTED_EDGE('',*,*,#6480,.F.);
#8851=ORIENTED_EDGE('',*,*,#6481,.F.);
#8852=ORIENTED_EDGE('',*,*,#6478,.F.);
#8853=ORIENTED_EDGE('',*,*,#6263,.F.);
#8854=ORIENTED_EDGE('',*,*,#6482,.F.);
#8855=ORIENTED_EDGE('',*,*,#6483,.F.);
#8856=ORIENTED_EDGE('',*,*,#6480,.T.);
#8857=ORIENTED_EDGE('',*,*,#6262,.F.);
#8858=ORIENTED_EDGE('',*,*,#6484,.F.);
#8859=ORIENTED_EDGE('',*,*,#6485,.F.);
#8860=ORIENTED_EDGE('',*,*,#6482,.T.);
#8861=ORIENTED_EDGE('',*,*,#6260,.F.);
#8862=ORIENTED_EDGE('',*,*,#6486,.F.);
#8863=ORIENTED_EDGE('',*,*,#6487,.F.);
#8864=ORIENTED_EDGE('',*,*,#6488,.F.);
#8865=ORIENTED_EDGE('',*,*,#6259,.F.);
#8866=ORIENTED_EDGE('',*,*,#6489,.F.);
#8867=ORIENTED_EDGE('',*,*,#6490,.F.);
#8868=ORIENTED_EDGE('',*,*,#6486,.T.);
#8869=ORIENTED_EDGE('',*,*,#6258,.F.);
#8870=ORIENTED_EDGE('',*,*,#6340,.F.);
#8871=ORIENTED_EDGE('',*,*,#6491,.F.);
#8872=ORIENTED_EDGE('',*,*,#6489,.T.);
#8873=ORIENTED_EDGE('',*,*,#6492,.T.);
#8874=ORIENTED_EDGE('',*,*,#6493,.T.);
#8875=ORIENTED_EDGE('',*,*,#6410,.T.);
#8876=ORIENTED_EDGE('',*,*,#6415,.F.);
#8877=ORIENTED_EDGE('',*,*,#6419,.T.);
#8878=ORIENTED_EDGE('',*,*,#6421,.T.);
#8879=ORIENTED_EDGE('',*,*,#6416,.T.);
#8880=ORIENTED_EDGE('',*,*,#6423,.F.);
#8881=ORIENTED_EDGE('',*,*,#6427,.T.);
#8882=ORIENTED_EDGE('',*,*,#6429,.T.);
#8883=ORIENTED_EDGE('',*,*,#6424,.T.);
#8884=ORIENTED_EDGE('',*,*,#6431,.F.);
#8885=ORIENTED_EDGE('',*,*,#6435,.T.);
#8886=ORIENTED_EDGE('',*,*,#6437,.T.);
#8887=ORIENTED_EDGE('',*,*,#6432,.T.);
#8888=ORIENTED_EDGE('',*,*,#6439,.F.);
#8889=ORIENTED_EDGE('',*,*,#6443,.T.);
#8890=ORIENTED_EDGE('',*,*,#6445,.T.);
#8891=ORIENTED_EDGE('',*,*,#6440,.T.);
#8892=ORIENTED_EDGE('',*,*,#6447,.F.);
#8893=ORIENTED_EDGE('',*,*,#6451,.T.);
#8894=ORIENTED_EDGE('',*,*,#6453,.T.);
#8895=ORIENTED_EDGE('',*,*,#6448,.T.);
#8896=ORIENTED_EDGE('',*,*,#6455,.F.);
#8897=ORIENTED_EDGE('',*,*,#6459,.T.);
#8898=ORIENTED_EDGE('',*,*,#6461,.T.);
#8899=ORIENTED_EDGE('',*,*,#6456,.T.);
#8900=ORIENTED_EDGE('',*,*,#6463,.F.);
#8901=ORIENTED_EDGE('',*,*,#6467,.T.);
#8902=ORIENTED_EDGE('',*,*,#6469,.T.);
#8903=ORIENTED_EDGE('',*,*,#6464,.T.);
#8904=ORIENTED_EDGE('',*,*,#6471,.F.);
#8905=ORIENTED_EDGE('',*,*,#6475,.T.);
#8906=ORIENTED_EDGE('',*,*,#6477,.T.);
#8907=ORIENTED_EDGE('',*,*,#6472,.T.);
#8908=ORIENTED_EDGE('',*,*,#6479,.F.);
#8909=ORIENTED_EDGE('',*,*,#6481,.T.);
#8910=ORIENTED_EDGE('',*,*,#6483,.T.);
#8911=ORIENTED_EDGE('',*,*,#6485,.T.);
#8912=ORIENTED_EDGE('',*,*,#6494,.F.);
#8913=ORIENTED_EDGE('',*,*,#6487,.T.);
#8914=ORIENTED_EDGE('',*,*,#6490,.T.);
#8915=ORIENTED_EDGE('',*,*,#6491,.T.);
#8916=ORIENTED_EDGE('',*,*,#6339,.F.);
#8917=ORIENTED_EDGE('',*,*,#6335,.T.);
#8918=ORIENTED_EDGE('',*,*,#6338,.T.);
#8919=ORIENTED_EDGE('',*,*,#6332,.T.);
#8920=ORIENTED_EDGE('',*,*,#6342,.F.);
#8921=ORIENTED_EDGE('',*,*,#6346,.T.);
#8922=ORIENTED_EDGE('',*,*,#6348,.T.);
#8923=ORIENTED_EDGE('',*,*,#6343,.T.);
#8924=ORIENTED_EDGE('',*,*,#6350,.F.);
#8925=ORIENTED_EDGE('',*,*,#6354,.T.);
#8926=ORIENTED_EDGE('',*,*,#6356,.T.);
#8927=ORIENTED_EDGE('',*,*,#6351,.T.);
#8928=ORIENTED_EDGE('',*,*,#6358,.F.);
#8929=ORIENTED_EDGE('',*,*,#6362,.T.);
#8930=ORIENTED_EDGE('',*,*,#6364,.T.);
#8931=ORIENTED_EDGE('',*,*,#6359,.T.);
#8932=ORIENTED_EDGE('',*,*,#6366,.F.);
#8933=ORIENTED_EDGE('',*,*,#6370,.T.);
#8934=ORIENTED_EDGE('',*,*,#6372,.T.);
#8935=ORIENTED_EDGE('',*,*,#6367,.T.);
#8936=ORIENTED_EDGE('',*,*,#6374,.F.);
#8937=ORIENTED_EDGE('',*,*,#6378,.T.);
#8938=ORIENTED_EDGE('',*,*,#6380,.T.);
#8939=ORIENTED_EDGE('',*,*,#6375,.T.);
#8940=ORIENTED_EDGE('',*,*,#6382,.F.);
#8941=ORIENTED_EDGE('',*,*,#6386,.T.);
#8942=ORIENTED_EDGE('',*,*,#6388,.T.);
#8943=ORIENTED_EDGE('',*,*,#6383,.T.);
#8944=ORIENTED_EDGE('',*,*,#6390,.F.);
#8945=ORIENTED_EDGE('',*,*,#6394,.T.);
#8946=ORIENTED_EDGE('',*,*,#6396,.T.);
#8947=ORIENTED_EDGE('',*,*,#6391,.T.);
#8948=ORIENTED_EDGE('',*,*,#6398,.F.);
#8949=ORIENTED_EDGE('',*,*,#6402,.T.);
#8950=ORIENTED_EDGE('',*,*,#6404,.T.);
#8951=ORIENTED_EDGE('',*,*,#6399,.T.);
#8952=ORIENTED_EDGE('',*,*,#6406,.F.);
#8953=ORIENTED_EDGE('',*,*,#6411,.T.);
#8954=ORIENTED_EDGE('',*,*,#6413,.T.);
#8955=ORIENTED_EDGE('',*,*,#6407,.T.);
#8956=ORIENTED_EDGE('',*,*,#6493,.F.);
#8957=ORIENTED_EDGE('',*,*,#6484,.T.);
#8958=ORIENTED_EDGE('',*,*,#6261,.F.);
#8959=ORIENTED_EDGE('',*,*,#6488,.T.);
#8960=ORIENTED_EDGE('',*,*,#6494,.T.);
#8961=ORIENTED_EDGE('',*,*,#6330,.T.);
#8962=ORIENTED_EDGE('',*,*,#6495,.F.);
#8963=ORIENTED_EDGE('',*,*,#6495,.T.);
#8964=ORIENTED_EDGE('',*,*,#6496,.T.);
#8965=ORIENTED_EDGE('',*,*,#6497,.F.);
#8966=ORIENTED_EDGE('',*,*,#6496,.F.);
#8967=ORIENTED_EDGE('',*,*,#6497,.T.);
#8968=ORIENTED_EDGE('',*,*,#6498,.T.);
#8969=ORIENTED_EDGE('',*,*,#6499,.F.);
#8970=ORIENTED_EDGE('',*,*,#6498,.F.);
#8971=ORIENTED_EDGE('',*,*,#6327,.T.);
#8972=ORIENTED_EDGE('',*,*,#6328,.T.);
#8973=ORIENTED_EDGE('',*,*,#6320,.T.);
#8974=ORIENTED_EDGE('',*,*,#6321,.T.);
#8975=ORIENTED_EDGE('',*,*,#6499,.T.);
#8976=ORIENTED_EDGE('',*,*,#6500,.T.);
#8977=ORIENTED_EDGE('',*,*,#6501,.F.);
#8978=ORIENTED_EDGE('',*,*,#6500,.F.);
#8979=ORIENTED_EDGE('',*,*,#6492,.F.);
#8980=ORIENTED_EDGE('',*,*,#6501,.T.);
#8981=ORIENTED_EDGE('',*,*,#6502,.T.);
#8982=ORIENTED_EDGE('',*,*,#6503,.T.);
#8983=ORIENTED_EDGE('',*,*,#6504,.T.);
#8984=ORIENTED_EDGE('',*,*,#6505,.T.);
#8985=ORIENTED_EDGE('',*,*,#6503,.F.);
#8986=ORIENTED_EDGE('',*,*,#6506,.F.);
#8987=ORIENTED_EDGE('',*,*,#6507,.T.);
#8988=ORIENTED_EDGE('',*,*,#6504,.F.);
#8989=ORIENTED_EDGE('',*,*,#6505,.F.);
#8990=ORIENTED_EDGE('',*,*,#6507,.F.);
#8991=ORIENTED_EDGE('',*,*,#6508,.T.);
#8992=ORIENTED_EDGE('',*,*,#6502,.F.);
#8993=ORIENTED_EDGE('',*,*,#6509,.T.);
#8994=ORIENTED_EDGE('',*,*,#6506,.T.);
#8995=ORIENTED_EDGE('',*,*,#6509,.F.);
#8996=ORIENTED_EDGE('',*,*,#6510,.F.);
#8997=ORIENTED_EDGE('',*,*,#6511,.T.);
#8998=ORIENTED_EDGE('',*,*,#6512,.F.);
#8999=ORIENTED_EDGE('',*,*,#6513,.T.);
#9000=ORIENTED_EDGE('',*,*,#6514,.F.);
#9001=ORIENTED_EDGE('',*,*,#6513,.F.);
#9002=ORIENTED_EDGE('',*,*,#6515,.F.);
#9003=ORIENTED_EDGE('',*,*,#6511,.F.);
#9004=ORIENTED_EDGE('',*,*,#6516,.F.);
#9005=ORIENTED_EDGE('',*,*,#6517,.F.);
#9006=ORIENTED_EDGE('',*,*,#6518,.F.);
#9007=ORIENTED_EDGE('',*,*,#6519,.T.);
#9008=ORIENTED_EDGE('',*,*,#6520,.F.);
#9009=ORIENTED_EDGE('',*,*,#6517,.T.);
#9010=ORIENTED_EDGE('',*,*,#6521,.F.);
#9011=ORIENTED_EDGE('',*,*,#6519,.F.);
#9012=ORIENTED_EDGE('',*,*,#6522,.F.);
#9013=ORIENTED_EDGE('',*,*,#6523,.F.);
#9014=ORIENTED_EDGE('',*,*,#6524,.T.);
#9015=ORIENTED_EDGE('',*,*,#6522,.T.);
#9016=ORIENTED_EDGE('',*,*,#6524,.F.);
#9017=ORIENTED_EDGE('',*,*,#6525,.F.);
#9018=ORIENTED_EDGE('',*,*,#6526,.T.);
#9019=ORIENTED_EDGE('',*,*,#6523,.T.);
#9020=ORIENTED_EDGE('',*,*,#6526,.F.);
#9021=ORIENTED_EDGE('',*,*,#6512,.T.);
#9022=ORIENTED_EDGE('',*,*,#6514,.T.);
#9023=ORIENTED_EDGE('',*,*,#6510,.T.);
#9024=ORIENTED_EDGE('',*,*,#6515,.T.);
#9025=ORIENTED_EDGE('',*,*,#6520,.T.);
#9026=ORIENTED_EDGE('',*,*,#6521,.T.);
#9027=ORIENTED_EDGE('',*,*,#6518,.T.);
#9028=ORIENTED_EDGE('',*,*,#6516,.T.);
#9029=ORIENTED_EDGE('',*,*,#6525,.T.);
#9030=ORIENTED_EDGE('',*,*,#6527,.F.);
#9031=ORIENTED_EDGE('',*,*,#6528,.F.);
#9032=ORIENTED_EDGE('',*,*,#6529,.T.);
#9033=ORIENTED_EDGE('',*,*,#6527,.T.);
#9034=ORIENTED_EDGE('',*,*,#6529,.F.);
#9035=ORIENTED_EDGE('',*,*,#6530,.F.);
#9036=ORIENTED_EDGE('',*,*,#6528,.T.);
#9037=ORIENTED_EDGE('',*,*,#6531,.F.);
#9038=ORIENTED_EDGE('',*,*,#6532,.T.);
#9039=ORIENTED_EDGE('',*,*,#6530,.T.);
#9040=ORIENTED_EDGE('',*,*,#6532,.F.);
#9041=ORIENTED_EDGE('',*,*,#6508,.F.);
#9042=ORIENTED_EDGE('',*,*,#6533,.T.);
#9043=ORIENTED_EDGE('',*,*,#6531,.T.);
#9044=ORIENTED_EDGE('',*,*,#6533,.F.);
#9045=ORIENTED_EDGE('',*,*,#6534,.F.);
#9046=ORIENTED_EDGE('',*,*,#6535,.T.);
#9047=ORIENTED_EDGE('',*,*,#6536,.T.);
#9048=ORIENTED_EDGE('',*,*,#6537,.T.);
#9049=ORIENTED_EDGE('',*,*,#6538,.T.);
#9050=ORIENTED_EDGE('',*,*,#6539,.T.);
#9051=ORIENTED_EDGE('',*,*,#6537,.F.);
#9052=ORIENTED_EDGE('',*,*,#6540,.T.);
#9053=ORIENTED_EDGE('',*,*,#6541,.T.);
#9054=ORIENTED_EDGE('',*,*,#6541,.F.);
#9055=ORIENTED_EDGE('',*,*,#6542,.F.);
#9056=ORIENTED_EDGE('',*,*,#6543,.F.);
#9057=ORIENTED_EDGE('',*,*,#6544,.F.);
#9058=ORIENTED_EDGE('',*,*,#6545,.T.);
#9059=ORIENTED_EDGE('',*,*,#6535,.F.);
#9060=ORIENTED_EDGE('',*,*,#6546,.T.);
#9061=ORIENTED_EDGE('',*,*,#6547,.F.);
#9062=ORIENTED_EDGE('',*,*,#6548,.F.);
#9063=ORIENTED_EDGE('',*,*,#6538,.F.);
#9064=ORIENTED_EDGE('',*,*,#6539,.F.);
#9065=ORIENTED_EDGE('',*,*,#6549,.T.);
#9066=ORIENTED_EDGE('',*,*,#6550,.F.);
#9067=ORIENTED_EDGE('',*,*,#6551,.F.);
#9068=ORIENTED_EDGE('',*,*,#6549,.F.);
#9069=ORIENTED_EDGE('',*,*,#6552,.F.);
#9070=ORIENTED_EDGE('',*,*,#6544,.T.);
#9071=ORIENTED_EDGE('',*,*,#6553,.T.);
#9072=ORIENTED_EDGE('',*,*,#6554,.T.);
#9073=ORIENTED_EDGE('',*,*,#6555,.T.);
#9074=ORIENTED_EDGE('',*,*,#6556,.T.);
#9075=ORIENTED_EDGE('',*,*,#6554,.F.);
#9076=ORIENTED_EDGE('',*,*,#6557,.T.);
#9077=ORIENTED_EDGE('',*,*,#6547,.T.);
#9078=ORIENTED_EDGE('',*,*,#6558,.F.);
#9079=ORIENTED_EDGE('',*,*,#6559,.F.);
#9080=ORIENTED_EDGE('',*,*,#6560,.T.);
#9081=ORIENTED_EDGE('',*,*,#6555,.F.);
#9082=ORIENTED_EDGE('',*,*,#6556,.F.);
#9083=ORIENTED_EDGE('',*,*,#6560,.F.);
#9084=ORIENTED_EDGE('',*,*,#6561,.F.);
#9085=ORIENTED_EDGE('',*,*,#6562,.T.);
#9086=ORIENTED_EDGE('',*,*,#6542,.T.);
#9087=ORIENTED_EDGE('',*,*,#6540,.F.);
#9088=ORIENTED_EDGE('',*,*,#6536,.F.);
#9089=ORIENTED_EDGE('',*,*,#6548,.T.);
#9090=ORIENTED_EDGE('',*,*,#6557,.F.);
#9091=ORIENTED_EDGE('',*,*,#6553,.F.);
#9092=ORIENTED_EDGE('',*,*,#6543,.T.);
#9093=ORIENTED_EDGE('',*,*,#6562,.F.);
#9094=ORIENTED_EDGE('',*,*,#6563,.F.);
#9095=ORIENTED_EDGE('',*,*,#6564,.T.);
#9096=ORIENTED_EDGE('',*,*,#6565,.F.);
#9097=ORIENTED_EDGE('',*,*,#6566,.F.);
#9098=ORIENTED_EDGE('',*,*,#6567,.F.);
#9099=ORIENTED_EDGE('',*,*,#6568,.F.);
#9100=ORIENTED_EDGE('',*,*,#6569,.F.);
#9101=ORIENTED_EDGE('',*,*,#6570,.F.);
#9102=ORIENTED_EDGE('',*,*,#6571,.F.);
#9103=ORIENTED_EDGE('',*,*,#6570,.T.);
#9104=ORIENTED_EDGE('',*,*,#6572,.F.);
#9105=ORIENTED_EDGE('',*,*,#6564,.F.);
#9106=ORIENTED_EDGE('',*,*,#6573,.F.);
#9107=ORIENTED_EDGE('',*,*,#6574,.T.);
#9108=ORIENTED_EDGE('',*,*,#6575,.T.);
#9109=ORIENTED_EDGE('',*,*,#6576,.T.);
#9110=ORIENTED_EDGE('',*,*,#6577,.T.);
#9111=ORIENTED_EDGE('',*,*,#6578,.T.);
#9112=ORIENTED_EDGE('',*,*,#6579,.T.);
#9113=ORIENTED_EDGE('',*,*,#6580,.T.);
#9114=ORIENTED_EDGE('',*,*,#6581,.T.);
#9115=ORIENTED_EDGE('',*,*,#6582,.T.);
#9116=ORIENTED_EDGE('',*,*,#6583,.T.);
#9117=ORIENTED_EDGE('',*,*,#6584,.T.);
#9118=ORIENTED_EDGE('',*,*,#6585,.T.);
#9119=ORIENTED_EDGE('',*,*,#6586,.T.);
#9120=ORIENTED_EDGE('',*,*,#6587,.T.);
#9121=ORIENTED_EDGE('',*,*,#6588,.T.);
#9122=ORIENTED_EDGE('',*,*,#6589,.T.);
#9123=ORIENTED_EDGE('',*,*,#6590,.T.);
#9124=ORIENTED_EDGE('',*,*,#6591,.T.);
#9125=ORIENTED_EDGE('',*,*,#6592,.T.);
#9126=ORIENTED_EDGE('',*,*,#6593,.T.);
#9127=ORIENTED_EDGE('',*,*,#6594,.T.);
#9128=ORIENTED_EDGE('',*,*,#6595,.T.);
#9129=ORIENTED_EDGE('',*,*,#6596,.T.);
#9130=ORIENTED_EDGE('',*,*,#6597,.T.);
#9131=ORIENTED_EDGE('',*,*,#6598,.T.);
#9132=ORIENTED_EDGE('',*,*,#6599,.T.);
#9133=ORIENTED_EDGE('',*,*,#6600,.T.);
#9134=ORIENTED_EDGE('',*,*,#6601,.T.);
#9135=ORIENTED_EDGE('',*,*,#6602,.T.);
#9136=ORIENTED_EDGE('',*,*,#6603,.T.);
#9137=ORIENTED_EDGE('',*,*,#6604,.T.);
#9138=ORIENTED_EDGE('',*,*,#6605,.T.);
#9139=ORIENTED_EDGE('',*,*,#6606,.T.);
#9140=ORIENTED_EDGE('',*,*,#6607,.T.);
#9141=ORIENTED_EDGE('',*,*,#6608,.T.);
#9142=ORIENTED_EDGE('',*,*,#6609,.T.);
#9143=ORIENTED_EDGE('',*,*,#6610,.T.);
#9144=ORIENTED_EDGE('',*,*,#6611,.T.);
#9145=ORIENTED_EDGE('',*,*,#6612,.T.);
#9146=ORIENTED_EDGE('',*,*,#6565,.T.);
#9147=ORIENTED_EDGE('',*,*,#6572,.T.);
#9148=ORIENTED_EDGE('',*,*,#6569,.T.);
#9149=ORIENTED_EDGE('',*,*,#6613,.T.);
#9150=ORIENTED_EDGE('',*,*,#6614,.T.);
#9151=ORIENTED_EDGE('',*,*,#6615,.T.);
#9152=ORIENTED_EDGE('',*,*,#6616,.T.);
#9153=ORIENTED_EDGE('',*,*,#6617,.T.);
#9154=ORIENTED_EDGE('',*,*,#6618,.T.);
#9155=ORIENTED_EDGE('',*,*,#6619,.T.);
#9156=ORIENTED_EDGE('',*,*,#6620,.T.);
#9157=ORIENTED_EDGE('',*,*,#6621,.T.);
#9158=ORIENTED_EDGE('',*,*,#6622,.T.);
#9159=ORIENTED_EDGE('',*,*,#6623,.T.);
#9160=ORIENTED_EDGE('',*,*,#6624,.T.);
#9161=ORIENTED_EDGE('',*,*,#6625,.T.);
#9162=ORIENTED_EDGE('',*,*,#6626,.T.);
#9163=ORIENTED_EDGE('',*,*,#6627,.T.);
#9164=ORIENTED_EDGE('',*,*,#6628,.T.);
#9165=ORIENTED_EDGE('',*,*,#6629,.T.);
#9166=ORIENTED_EDGE('',*,*,#6630,.T.);
#9167=ORIENTED_EDGE('',*,*,#6631,.T.);
#9168=ORIENTED_EDGE('',*,*,#6632,.T.);
#9169=ORIENTED_EDGE('',*,*,#6633,.T.);
#9170=ORIENTED_EDGE('',*,*,#6634,.T.);
#9171=ORIENTED_EDGE('',*,*,#6635,.T.);
#9172=ORIENTED_EDGE('',*,*,#6636,.T.);
#9173=ORIENTED_EDGE('',*,*,#6637,.T.);
#9174=ORIENTED_EDGE('',*,*,#6638,.T.);
#9175=ORIENTED_EDGE('',*,*,#6639,.T.);
#9176=ORIENTED_EDGE('',*,*,#6640,.T.);
#9177=ORIENTED_EDGE('',*,*,#6641,.T.);
#9178=ORIENTED_EDGE('',*,*,#6642,.T.);
#9179=ORIENTED_EDGE('',*,*,#6643,.T.);
#9180=ORIENTED_EDGE('',*,*,#6644,.T.);
#9181=ORIENTED_EDGE('',*,*,#6645,.T.);
#9182=ORIENTED_EDGE('',*,*,#6646,.T.);
#9183=ORIENTED_EDGE('',*,*,#6647,.T.);
#9184=ORIENTED_EDGE('',*,*,#6648,.T.);
#9185=ORIENTED_EDGE('',*,*,#6649,.T.);
#9186=ORIENTED_EDGE('',*,*,#6650,.T.);
#9187=ORIENTED_EDGE('',*,*,#6651,.T.);
#9188=ORIENTED_EDGE('',*,*,#6652,.T.);
#9189=ORIENTED_EDGE('',*,*,#6574,.F.);
#9190=ORIENTED_EDGE('',*,*,#6568,.T.);
#9191=ORIENTED_EDGE('',*,*,#6653,.T.);
#9192=ORIENTED_EDGE('',*,*,#6654,.T.);
#9193=ORIENTED_EDGE('',*,*,#6613,.F.);
#9194=ORIENTED_EDGE('',*,*,#6566,.T.);
#9195=ORIENTED_EDGE('',*,*,#6612,.F.);
#9196=ORIENTED_EDGE('',*,*,#6655,.T.);
#9197=ORIENTED_EDGE('',*,*,#6656,.T.);
#9198=ORIENTED_EDGE('',*,*,#6657,.F.);
#9199=ORIENTED_EDGE('',*,*,#6658,.T.);
#9200=ORIENTED_EDGE('',*,*,#6609,.F.);
#9201=ORIENTED_EDGE('',*,*,#6659,.F.);
#9202=ORIENTED_EDGE('',*,*,#6660,.F.);
#9203=ORIENTED_EDGE('',*,*,#6655,.F.);
#9204=ORIENTED_EDGE('',*,*,#6611,.F.);
#9205=ORIENTED_EDGE('',*,*,#6661,.F.);
#9206=ORIENTED_EDGE('',*,*,#6662,.F.);
#9207=ORIENTED_EDGE('',*,*,#6661,.T.);
#9208=ORIENTED_EDGE('',*,*,#6610,.F.);
#9209=ORIENTED_EDGE('',*,*,#6658,.F.);
#9210=ORIENTED_EDGE('',*,*,#6659,.T.);
#9211=ORIENTED_EDGE('',*,*,#6608,.F.);
#9212=ORIENTED_EDGE('',*,*,#6663,.T.);
#9213=ORIENTED_EDGE('',*,*,#6664,.T.);
#9214=ORIENTED_EDGE('',*,*,#6665,.F.);
#9215=ORIENTED_EDGE('',*,*,#6666,.T.);
#9216=ORIENTED_EDGE('',*,*,#6605,.F.);
#9217=ORIENTED_EDGE('',*,*,#6667,.F.);
#9218=ORIENTED_EDGE('',*,*,#6668,.F.);
#9219=ORIENTED_EDGE('',*,*,#6663,.F.);
#9220=ORIENTED_EDGE('',*,*,#6607,.F.);
#9221=ORIENTED_EDGE('',*,*,#6669,.F.);
#9222=ORIENTED_EDGE('',*,*,#6670,.F.);
#9223=ORIENTED_EDGE('',*,*,#6669,.T.);
#9224=ORIENTED_EDGE('',*,*,#6606,.F.);
#9225=ORIENTED_EDGE('',*,*,#6666,.F.);
#9226=ORIENTED_EDGE('',*,*,#6667,.T.);
#9227=ORIENTED_EDGE('',*,*,#6604,.F.);
#9228=ORIENTED_EDGE('',*,*,#6671,.T.);
#9229=ORIENTED_EDGE('',*,*,#6672,.T.);
#9230=ORIENTED_EDGE('',*,*,#6673,.F.);
#9231=ORIENTED_EDGE('',*,*,#6674,.T.);
#9232=ORIENTED_EDGE('',*,*,#6601,.F.);
#9233=ORIENTED_EDGE('',*,*,#6675,.F.);
#9234=ORIENTED_EDGE('',*,*,#6676,.F.);
#9235=ORIENTED_EDGE('',*,*,#6671,.F.);
#9236=ORIENTED_EDGE('',*,*,#6603,.F.);
#9237=ORIENTED_EDGE('',*,*,#6677,.F.);
#9238=ORIENTED_EDGE('',*,*,#6678,.F.);
#9239=ORIENTED_EDGE('',*,*,#6677,.T.);
#9240=ORIENTED_EDGE('',*,*,#6602,.F.);
#9241=ORIENTED_EDGE('',*,*,#6674,.F.);
#9242=ORIENTED_EDGE('',*,*,#6675,.T.);
#9243=ORIENTED_EDGE('',*,*,#6600,.F.);
#9244=ORIENTED_EDGE('',*,*,#6679,.T.);
#9245=ORIENTED_EDGE('',*,*,#6680,.T.);
#9246=ORIENTED_EDGE('',*,*,#6681,.F.);
#9247=ORIENTED_EDGE('',*,*,#6682,.T.);
#9248=ORIENTED_EDGE('',*,*,#6597,.F.);
#9249=ORIENTED_EDGE('',*,*,#6683,.F.);
#9250=ORIENTED_EDGE('',*,*,#6684,.F.);
#9251=ORIENTED_EDGE('',*,*,#6679,.F.);
#9252=ORIENTED_EDGE('',*,*,#6599,.F.);
#9253=ORIENTED_EDGE('',*,*,#6685,.F.);
#9254=ORIENTED_EDGE('',*,*,#6686,.F.);
#9255=ORIENTED_EDGE('',*,*,#6685,.T.);
#9256=ORIENTED_EDGE('',*,*,#6598,.F.);
#9257=ORIENTED_EDGE('',*,*,#6682,.F.);
#9258=ORIENTED_EDGE('',*,*,#6683,.T.);
#9259=ORIENTED_EDGE('',*,*,#6596,.F.);
#9260=ORIENTED_EDGE('',*,*,#6687,.T.);
#9261=ORIENTED_EDGE('',*,*,#6688,.T.);
#9262=ORIENTED_EDGE('',*,*,#6689,.F.);
#9263=ORIENTED_EDGE('',*,*,#6690,.T.);
#9264=ORIENTED_EDGE('',*,*,#6593,.F.);
#9265=ORIENTED_EDGE('',*,*,#6691,.F.);
#9266=ORIENTED_EDGE('',*,*,#6692,.F.);
#9267=ORIENTED_EDGE('',*,*,#6687,.F.);
#9268=ORIENTED_EDGE('',*,*,#6595,.F.);
#9269=ORIENTED_EDGE('',*,*,#6693,.F.);
#9270=ORIENTED_EDGE('',*,*,#6694,.F.);
#9271=ORIENTED_EDGE('',*,*,#6693,.T.);
#9272=ORIENTED_EDGE('',*,*,#6594,.F.);
#9273=ORIENTED_EDGE('',*,*,#6690,.F.);
#9274=ORIENTED_EDGE('',*,*,#6691,.T.);
#9275=ORIENTED_EDGE('',*,*,#6592,.F.);
#9276=ORIENTED_EDGE('',*,*,#6695,.T.);
#9277=ORIENTED_EDGE('',*,*,#6696,.T.);
#9278=ORIENTED_EDGE('',*,*,#6697,.F.);
#9279=ORIENTED_EDGE('',*,*,#6698,.T.);
#9280=ORIENTED_EDGE('',*,*,#6589,.F.);
#9281=ORIENTED_EDGE('',*,*,#6699,.F.);
#9282=ORIENTED_EDGE('',*,*,#6700,.F.);
#9283=ORIENTED_EDGE('',*,*,#6695,.F.);
#9284=ORIENTED_EDGE('',*,*,#6591,.F.);
#9285=ORIENTED_EDGE('',*,*,#6701,.F.);
#9286=ORIENTED_EDGE('',*,*,#6702,.F.);
#9287=ORIENTED_EDGE('',*,*,#6701,.T.);
#9288=ORIENTED_EDGE('',*,*,#6590,.F.);
#9289=ORIENTED_EDGE('',*,*,#6698,.F.);
#9290=ORIENTED_EDGE('',*,*,#6699,.T.);
#9291=ORIENTED_EDGE('',*,*,#6588,.F.);
#9292=ORIENTED_EDGE('',*,*,#6703,.T.);
#9293=ORIENTED_EDGE('',*,*,#6704,.T.);
#9294=ORIENTED_EDGE('',*,*,#6705,.F.);
#9295=ORIENTED_EDGE('',*,*,#6706,.T.);
#9296=ORIENTED_EDGE('',*,*,#6585,.F.);
#9297=ORIENTED_EDGE('',*,*,#6707,.F.);
#9298=ORIENTED_EDGE('',*,*,#6708,.F.);
#9299=ORIENTED_EDGE('',*,*,#6703,.F.);
#9300=ORIENTED_EDGE('',*,*,#6587,.F.);
#9301=ORIENTED_EDGE('',*,*,#6709,.F.);
#9302=ORIENTED_EDGE('',*,*,#6710,.F.);
#9303=ORIENTED_EDGE('',*,*,#6709,.T.);
#9304=ORIENTED_EDGE('',*,*,#6586,.F.);
#9305=ORIENTED_EDGE('',*,*,#6706,.F.);
#9306=ORIENTED_EDGE('',*,*,#6707,.T.);
#9307=ORIENTED_EDGE('',*,*,#6584,.F.);
#9308=ORIENTED_EDGE('',*,*,#6711,.T.);
#9309=ORIENTED_EDGE('',*,*,#6712,.T.);
#9310=ORIENTED_EDGE('',*,*,#6713,.F.);
#9311=ORIENTED_EDGE('',*,*,#6714,.T.);
#9312=ORIENTED_EDGE('',*,*,#6581,.F.);
#9313=ORIENTED_EDGE('',*,*,#6715,.F.);
#9314=ORIENTED_EDGE('',*,*,#6716,.F.);
#9315=ORIENTED_EDGE('',*,*,#6711,.F.);
#9316=ORIENTED_EDGE('',*,*,#6583,.F.);
#9317=ORIENTED_EDGE('',*,*,#6717,.F.);
#9318=ORIENTED_EDGE('',*,*,#6718,.F.);
#9319=ORIENTED_EDGE('',*,*,#6717,.T.);
#9320=ORIENTED_EDGE('',*,*,#6582,.F.);
#9321=ORIENTED_EDGE('',*,*,#6714,.F.);
#9322=ORIENTED_EDGE('',*,*,#6715,.T.);
#9323=ORIENTED_EDGE('',*,*,#6580,.F.);
#9324=ORIENTED_EDGE('',*,*,#6719,.T.);
#9325=ORIENTED_EDGE('',*,*,#6720,.T.);
#9326=ORIENTED_EDGE('',*,*,#6721,.F.);
#9327=ORIENTED_EDGE('',*,*,#6722,.T.);
#9328=ORIENTED_EDGE('',*,*,#6577,.F.);
#9329=ORIENTED_EDGE('',*,*,#6723,.F.);
#9330=ORIENTED_EDGE('',*,*,#6724,.F.);
#9331=ORIENTED_EDGE('',*,*,#6719,.F.);
#9332=ORIENTED_EDGE('',*,*,#6579,.F.);
#9333=ORIENTED_EDGE('',*,*,#6725,.F.);
#9334=ORIENTED_EDGE('',*,*,#6726,.F.);
#9335=ORIENTED_EDGE('',*,*,#6727,.F.);
#9336=ORIENTED_EDGE('',*,*,#6725,.T.);
#9337=ORIENTED_EDGE('',*,*,#6578,.F.);
#9338=ORIENTED_EDGE('',*,*,#6722,.F.);
#9339=ORIENTED_EDGE('',*,*,#6723,.T.);
#9340=ORIENTED_EDGE('',*,*,#6576,.F.);
#9341=ORIENTED_EDGE('',*,*,#6728,.T.);
#9342=ORIENTED_EDGE('',*,*,#6729,.T.);
#9343=ORIENTED_EDGE('',*,*,#6730,.F.);
#9344=ORIENTED_EDGE('',*,*,#6731,.T.);
#9345=ORIENTED_EDGE('',*,*,#6650,.F.);
#9346=ORIENTED_EDGE('',*,*,#6732,.F.);
#9347=ORIENTED_EDGE('',*,*,#6733,.F.);
#9348=ORIENTED_EDGE('',*,*,#6728,.F.);
#9349=ORIENTED_EDGE('',*,*,#6575,.F.);
#9350=ORIENTED_EDGE('',*,*,#6652,.F.);
#9351=ORIENTED_EDGE('',*,*,#6734,.F.);
#9352=ORIENTED_EDGE('',*,*,#6735,.F.);
#9353=ORIENTED_EDGE('',*,*,#6734,.T.);
#9354=ORIENTED_EDGE('',*,*,#6651,.F.);
#9355=ORIENTED_EDGE('',*,*,#6731,.F.);
#9356=ORIENTED_EDGE('',*,*,#6732,.T.);
#9357=ORIENTED_EDGE('',*,*,#6649,.F.);
#9358=ORIENTED_EDGE('',*,*,#6736,.T.);
#9359=ORIENTED_EDGE('',*,*,#6737,.T.);
#9360=ORIENTED_EDGE('',*,*,#6738,.F.);
#9361=ORIENTED_EDGE('',*,*,#6739,.T.);
#9362=ORIENTED_EDGE('',*,*,#6646,.F.);
#9363=ORIENTED_EDGE('',*,*,#6740,.F.);
#9364=ORIENTED_EDGE('',*,*,#6741,.F.);
#9365=ORIENTED_EDGE('',*,*,#6736,.F.);
#9366=ORIENTED_EDGE('',*,*,#6648,.F.);
#9367=ORIENTED_EDGE('',*,*,#6742,.F.);
#9368=ORIENTED_EDGE('',*,*,#6743,.F.);
#9369=ORIENTED_EDGE('',*,*,#6742,.T.);
#9370=ORIENTED_EDGE('',*,*,#6647,.F.);
#9371=ORIENTED_EDGE('',*,*,#6739,.F.);
#9372=ORIENTED_EDGE('',*,*,#6740,.T.);
#9373=ORIENTED_EDGE('',*,*,#6645,.F.);
#9374=ORIENTED_EDGE('',*,*,#6744,.T.);
#9375=ORIENTED_EDGE('',*,*,#6745,.T.);
#9376=ORIENTED_EDGE('',*,*,#6746,.F.);
#9377=ORIENTED_EDGE('',*,*,#6747,.T.);
#9378=ORIENTED_EDGE('',*,*,#6642,.F.);
#9379=ORIENTED_EDGE('',*,*,#6748,.F.);
#9380=ORIENTED_EDGE('',*,*,#6749,.F.);
#9381=ORIENTED_EDGE('',*,*,#6744,.F.);
#9382=ORIENTED_EDGE('',*,*,#6644,.F.);
#9383=ORIENTED_EDGE('',*,*,#6750,.F.);
#9384=ORIENTED_EDGE('',*,*,#6751,.F.);
#9385=ORIENTED_EDGE('',*,*,#6750,.T.);
#9386=ORIENTED_EDGE('',*,*,#6643,.F.);
#9387=ORIENTED_EDGE('',*,*,#6747,.F.);
#9388=ORIENTED_EDGE('',*,*,#6748,.T.);
#9389=ORIENTED_EDGE('',*,*,#6641,.F.);
#9390=ORIENTED_EDGE('',*,*,#6752,.T.);
#9391=ORIENTED_EDGE('',*,*,#6753,.T.);
#9392=ORIENTED_EDGE('',*,*,#6754,.F.);
#9393=ORIENTED_EDGE('',*,*,#6755,.T.);
#9394=ORIENTED_EDGE('',*,*,#6638,.F.);
#9395=ORIENTED_EDGE('',*,*,#6756,.F.);
#9396=ORIENTED_EDGE('',*,*,#6757,.F.);
#9397=ORIENTED_EDGE('',*,*,#6752,.F.);
#9398=ORIENTED_EDGE('',*,*,#6640,.F.);
#9399=ORIENTED_EDGE('',*,*,#6758,.F.);
#9400=ORIENTED_EDGE('',*,*,#6759,.F.);
#9401=ORIENTED_EDGE('',*,*,#6758,.T.);
#9402=ORIENTED_EDGE('',*,*,#6639,.F.);
#9403=ORIENTED_EDGE('',*,*,#6755,.F.);
#9404=ORIENTED_EDGE('',*,*,#6756,.T.);
#9405=ORIENTED_EDGE('',*,*,#6637,.F.);
#9406=ORIENTED_EDGE('',*,*,#6760,.T.);
#9407=ORIENTED_EDGE('',*,*,#6761,.T.);
#9408=ORIENTED_EDGE('',*,*,#6762,.F.);
#9409=ORIENTED_EDGE('',*,*,#6763,.T.);
#9410=ORIENTED_EDGE('',*,*,#6634,.F.);
#9411=ORIENTED_EDGE('',*,*,#6764,.F.);
#9412=ORIENTED_EDGE('',*,*,#6765,.F.);
#9413=ORIENTED_EDGE('',*,*,#6760,.F.);
#9414=ORIENTED_EDGE('',*,*,#6636,.F.);
#9415=ORIENTED_EDGE('',*,*,#6766,.F.);
#9416=ORIENTED_EDGE('',*,*,#6767,.F.);
#9417=ORIENTED_EDGE('',*,*,#6766,.T.);
#9418=ORIENTED_EDGE('',*,*,#6635,.F.);
#9419=ORIENTED_EDGE('',*,*,#6763,.F.);
#9420=ORIENTED_EDGE('',*,*,#6764,.T.);
#9421=ORIENTED_EDGE('',*,*,#6633,.F.);
#9422=ORIENTED_EDGE('',*,*,#6768,.T.);
#9423=ORIENTED_EDGE('',*,*,#6769,.T.);
#9424=ORIENTED_EDGE('',*,*,#6770,.F.);
#9425=ORIENTED_EDGE('',*,*,#6771,.T.);
#9426=ORIENTED_EDGE('',*,*,#6630,.F.);
#9427=ORIENTED_EDGE('',*,*,#6772,.F.);
#9428=ORIENTED_EDGE('',*,*,#6773,.F.);
#9429=ORIENTED_EDGE('',*,*,#6768,.F.);
#9430=ORIENTED_EDGE('',*,*,#6632,.F.);
#9431=ORIENTED_EDGE('',*,*,#6774,.F.);
#9432=ORIENTED_EDGE('',*,*,#6775,.F.);
#9433=ORIENTED_EDGE('',*,*,#6774,.T.);
#9434=ORIENTED_EDGE('',*,*,#6631,.F.);
#9435=ORIENTED_EDGE('',*,*,#6771,.F.);
#9436=ORIENTED_EDGE('',*,*,#6772,.T.);
#9437=ORIENTED_EDGE('',*,*,#6629,.F.);
#9438=ORIENTED_EDGE('',*,*,#6776,.T.);
#9439=ORIENTED_EDGE('',*,*,#6777,.T.);
#9440=ORIENTED_EDGE('',*,*,#6778,.F.);
#9441=ORIENTED_EDGE('',*,*,#6779,.T.);
#9442=ORIENTED_EDGE('',*,*,#6626,.F.);
#9443=ORIENTED_EDGE('',*,*,#6780,.F.);
#9444=ORIENTED_EDGE('',*,*,#6781,.F.);
#9445=ORIENTED_EDGE('',*,*,#6776,.F.);
#9446=ORIENTED_EDGE('',*,*,#6628,.F.);
#9447=ORIENTED_EDGE('',*,*,#6782,.F.);
#9448=ORIENTED_EDGE('',*,*,#6783,.F.);
#9449=ORIENTED_EDGE('',*,*,#6782,.T.);
#9450=ORIENTED_EDGE('',*,*,#6627,.F.);
#9451=ORIENTED_EDGE('',*,*,#6779,.F.);
#9452=ORIENTED_EDGE('',*,*,#6780,.T.);
#9453=ORIENTED_EDGE('',*,*,#6625,.F.);
#9454=ORIENTED_EDGE('',*,*,#6784,.T.);
#9455=ORIENTED_EDGE('',*,*,#6785,.T.);
#9456=ORIENTED_EDGE('',*,*,#6786,.F.);
#9457=ORIENTED_EDGE('',*,*,#6787,.T.);
#9458=ORIENTED_EDGE('',*,*,#6622,.F.);
#9459=ORIENTED_EDGE('',*,*,#6788,.F.);
#9460=ORIENTED_EDGE('',*,*,#6789,.F.);
#9461=ORIENTED_EDGE('',*,*,#6784,.F.);
#9462=ORIENTED_EDGE('',*,*,#6624,.F.);
#9463=ORIENTED_EDGE('',*,*,#6790,.F.);
#9464=ORIENTED_EDGE('',*,*,#6791,.F.);
#9465=ORIENTED_EDGE('',*,*,#6790,.T.);
#9466=ORIENTED_EDGE('',*,*,#6623,.F.);
#9467=ORIENTED_EDGE('',*,*,#6787,.F.);
#9468=ORIENTED_EDGE('',*,*,#6788,.T.);
#9469=ORIENTED_EDGE('',*,*,#6621,.F.);
#9470=ORIENTED_EDGE('',*,*,#6792,.T.);
#9471=ORIENTED_EDGE('',*,*,#6793,.T.);
#9472=ORIENTED_EDGE('',*,*,#6620,.F.);
#9473=ORIENTED_EDGE('',*,*,#6794,.F.);
#9474=ORIENTED_EDGE('',*,*,#6795,.F.);
#9475=ORIENTED_EDGE('',*,*,#6792,.F.);
#9476=ORIENTED_EDGE('',*,*,#6619,.F.);
#9477=ORIENTED_EDGE('',*,*,#6796,.F.);
#9478=ORIENTED_EDGE('',*,*,#6797,.F.);
#9479=ORIENTED_EDGE('',*,*,#6794,.T.);
#9480=ORIENTED_EDGE('',*,*,#6618,.F.);
#9481=ORIENTED_EDGE('',*,*,#6798,.F.);
#9482=ORIENTED_EDGE('',*,*,#6799,.F.);
#9483=ORIENTED_EDGE('',*,*,#6796,.T.);
#9484=ORIENTED_EDGE('',*,*,#6616,.F.);
#9485=ORIENTED_EDGE('',*,*,#6800,.F.);
#9486=ORIENTED_EDGE('',*,*,#6801,.F.);
#9487=ORIENTED_EDGE('',*,*,#6802,.F.);
#9488=ORIENTED_EDGE('',*,*,#6615,.F.);
#9489=ORIENTED_EDGE('',*,*,#6803,.F.);
#9490=ORIENTED_EDGE('',*,*,#6804,.F.);
#9491=ORIENTED_EDGE('',*,*,#6800,.T.);
#9492=ORIENTED_EDGE('',*,*,#6614,.F.);
#9493=ORIENTED_EDGE('',*,*,#6654,.F.);
#9494=ORIENTED_EDGE('',*,*,#6805,.F.);
#9495=ORIENTED_EDGE('',*,*,#6803,.T.);
#9496=ORIENTED_EDGE('',*,*,#6806,.T.);
#9497=ORIENTED_EDGE('',*,*,#6807,.T.);
#9498=ORIENTED_EDGE('',*,*,#6726,.T.);
#9499=ORIENTED_EDGE('',*,*,#6727,.T.);
#9500=ORIENTED_EDGE('',*,*,#6721,.T.);
#9501=ORIENTED_EDGE('',*,*,#6729,.F.);
#9502=ORIENTED_EDGE('',*,*,#6733,.T.);
#9503=ORIENTED_EDGE('',*,*,#6735,.T.);
#9504=ORIENTED_EDGE('',*,*,#6730,.T.);
#9505=ORIENTED_EDGE('',*,*,#6737,.F.);
#9506=ORIENTED_EDGE('',*,*,#6741,.T.);
#9507=ORIENTED_EDGE('',*,*,#6743,.T.);
#9508=ORIENTED_EDGE('',*,*,#6738,.T.);
#9509=ORIENTED_EDGE('',*,*,#6745,.F.);
#9510=ORIENTED_EDGE('',*,*,#6749,.T.);
#9511=ORIENTED_EDGE('',*,*,#6751,.T.);
#9512=ORIENTED_EDGE('',*,*,#6746,.T.);
#9513=ORIENTED_EDGE('',*,*,#6753,.F.);
#9514=ORIENTED_EDGE('',*,*,#6757,.T.);
#9515=ORIENTED_EDGE('',*,*,#6759,.T.);
#9516=ORIENTED_EDGE('',*,*,#6754,.T.);
#9517=ORIENTED_EDGE('',*,*,#6761,.F.);
#9518=ORIENTED_EDGE('',*,*,#6765,.T.);
#9519=ORIENTED_EDGE('',*,*,#6767,.T.);
#9520=ORIENTED_EDGE('',*,*,#6762,.T.);
#9521=ORIENTED_EDGE('',*,*,#6769,.F.);
#9522=ORIENTED_EDGE('',*,*,#6773,.T.);
#9523=ORIENTED_EDGE('',*,*,#6775,.T.);
#9524=ORIENTED_EDGE('',*,*,#6770,.T.);
#9525=ORIENTED_EDGE('',*,*,#6777,.F.);
#9526=ORIENTED_EDGE('',*,*,#6781,.T.);
#9527=ORIENTED_EDGE('',*,*,#6783,.T.);
#9528=ORIENTED_EDGE('',*,*,#6778,.T.);
#9529=ORIENTED_EDGE('',*,*,#6785,.F.);
#9530=ORIENTED_EDGE('',*,*,#6789,.T.);
#9531=ORIENTED_EDGE('',*,*,#6791,.T.);
#9532=ORIENTED_EDGE('',*,*,#6786,.T.);
#9533=ORIENTED_EDGE('',*,*,#6793,.F.);
#9534=ORIENTED_EDGE('',*,*,#6795,.T.);
#9535=ORIENTED_EDGE('',*,*,#6797,.T.);
#9536=ORIENTED_EDGE('',*,*,#6799,.T.);
#9537=ORIENTED_EDGE('',*,*,#6808,.F.);
#9538=ORIENTED_EDGE('',*,*,#6801,.T.);
#9539=ORIENTED_EDGE('',*,*,#6804,.T.);
#9540=ORIENTED_EDGE('',*,*,#6805,.T.);
#9541=ORIENTED_EDGE('',*,*,#6653,.F.);
#9542=ORIENTED_EDGE('',*,*,#6567,.T.);
#9543=ORIENTED_EDGE('',*,*,#6571,.T.);
#9544=ORIENTED_EDGE('',*,*,#6563,.T.);
#9545=ORIENTED_EDGE('',*,*,#6656,.F.);
#9546=ORIENTED_EDGE('',*,*,#6660,.T.);
#9547=ORIENTED_EDGE('',*,*,#6662,.T.);
#9548=ORIENTED_EDGE('',*,*,#6657,.T.);
#9549=ORIENTED_EDGE('',*,*,#6664,.F.);
#9550=ORIENTED_EDGE('',*,*,#6668,.T.);
#9551=ORIENTED_EDGE('',*,*,#6670,.T.);
#9552=ORIENTED_EDGE('',*,*,#6665,.T.);
#9553=ORIENTED_EDGE('',*,*,#6672,.F.);
#9554=ORIENTED_EDGE('',*,*,#6676,.T.);
#9555=ORIENTED_EDGE('',*,*,#6678,.T.);
#9556=ORIENTED_EDGE('',*,*,#6673,.T.);
#9557=ORIENTED_EDGE('',*,*,#6680,.F.);
#9558=ORIENTED_EDGE('',*,*,#6684,.T.);
#9559=ORIENTED_EDGE('',*,*,#6686,.T.);
#9560=ORIENTED_EDGE('',*,*,#6681,.T.);
#9561=ORIENTED_EDGE('',*,*,#6688,.F.);
#9562=ORIENTED_EDGE('',*,*,#6692,.T.);
#9563=ORIENTED_EDGE('',*,*,#6694,.T.);
#9564=ORIENTED_EDGE('',*,*,#6689,.T.);
#9565=ORIENTED_EDGE('',*,*,#6696,.F.);
#9566=ORIENTED_EDGE('',*,*,#6700,.T.);
#9567=ORIENTED_EDGE('',*,*,#6702,.T.);
#9568=ORIENTED_EDGE('',*,*,#6697,.T.);
#9569=ORIENTED_EDGE('',*,*,#6704,.F.);
#9570=ORIENTED_EDGE('',*,*,#6708,.T.);
#9571=ORIENTED_EDGE('',*,*,#6710,.T.);
#9572=ORIENTED_EDGE('',*,*,#6705,.T.);
#9573=ORIENTED_EDGE('',*,*,#6712,.F.);
#9574=ORIENTED_EDGE('',*,*,#6716,.T.);
#9575=ORIENTED_EDGE('',*,*,#6718,.T.);
#9576=ORIENTED_EDGE('',*,*,#6713,.T.);
#9577=ORIENTED_EDGE('',*,*,#6720,.F.);
#9578=ORIENTED_EDGE('',*,*,#6724,.T.);
#9579=ORIENTED_EDGE('',*,*,#6807,.F.);
#9580=ORIENTED_EDGE('',*,*,#6798,.T.);
#9581=ORIENTED_EDGE('',*,*,#6617,.F.);
#9582=ORIENTED_EDGE('',*,*,#6802,.T.);
#9583=ORIENTED_EDGE('',*,*,#6808,.T.);
#9584=ORIENTED_EDGE('',*,*,#6573,.T.);
#9585=ORIENTED_EDGE('',*,*,#6545,.F.);
#9586=ORIENTED_EDGE('',*,*,#6552,.T.);
#9587=ORIENTED_EDGE('',*,*,#6546,.F.);
#9588=ORIENTED_EDGE('',*,*,#6534,.T.);
#9589=ORIENTED_EDGE('',*,*,#6561,.T.);
#9590=ORIENTED_EDGE('',*,*,#6809,.F.);
#9591=ORIENTED_EDGE('',*,*,#6809,.T.);
#9592=ORIENTED_EDGE('',*,*,#6810,.T.);
#9593=ORIENTED_EDGE('',*,*,#6811,.F.);
#9594=ORIENTED_EDGE('',*,*,#6810,.F.);
#9595=ORIENTED_EDGE('',*,*,#6811,.T.);
#9596=ORIENTED_EDGE('',*,*,#6812,.T.);
#9597=ORIENTED_EDGE('',*,*,#6813,.F.);
#9598=ORIENTED_EDGE('',*,*,#6812,.F.);
#9599=ORIENTED_EDGE('',*,*,#6558,.T.);
#9600=ORIENTED_EDGE('',*,*,#6559,.T.);
#9601=ORIENTED_EDGE('',*,*,#6550,.T.);
#9602=ORIENTED_EDGE('',*,*,#6551,.T.);
#9603=ORIENTED_EDGE('',*,*,#6813,.T.);
#9604=ORIENTED_EDGE('',*,*,#6814,.T.);
#9605=ORIENTED_EDGE('',*,*,#6815,.F.);
#9606=ORIENTED_EDGE('',*,*,#6814,.F.);
#9607=ORIENTED_EDGE('',*,*,#6806,.F.);
#9608=ORIENTED_EDGE('',*,*,#6815,.T.);
#9609=ORIENTED_EDGE('',*,*,#6816,.F.);
#9610=ORIENTED_EDGE('',*,*,#6817,.T.);
#9611=ORIENTED_EDGE('',*,*,#6818,.F.);
#9612=ORIENTED_EDGE('',*,*,#6819,.F.);
#9613=ORIENTED_EDGE('',*,*,#6819,.T.);
#9614=ORIENTED_EDGE('',*,*,#6820,.T.);
#9615=ORIENTED_EDGE('',*,*,#6817,.F.);
#9616=ORIENTED_EDGE('',*,*,#6820,.F.);
#9617=ORIENTED_EDGE('',*,*,#6821,.T.);
#9618=ORIENTED_EDGE('',*,*,#6822,.T.);
#9619=ORIENTED_EDGE('',*,*,#6818,.T.);
#9620=ORIENTED_EDGE('',*,*,#6822,.F.);
#9621=ORIENTED_EDGE('',*,*,#6823,.F.);
#9622=ORIENTED_EDGE('',*,*,#6824,.T.);
#9623=ORIENTED_EDGE('',*,*,#6825,.F.);
#9624=ORIENTED_EDGE('',*,*,#6826,.F.);
#9625=ORIENTED_EDGE('',*,*,#6826,.T.);
#9626=ORIENTED_EDGE('',*,*,#6827,.T.);
#9627=ORIENTED_EDGE('',*,*,#6824,.F.);
#9628=ORIENTED_EDGE('',*,*,#6827,.F.);
#9629=ORIENTED_EDGE('',*,*,#6828,.T.);
#9630=ORIENTED_EDGE('',*,*,#6829,.T.);
#9631=ORIENTED_EDGE('',*,*,#6830,.T.);
#9632=ORIENTED_EDGE('',*,*,#6831,.T.);
#9633=ORIENTED_EDGE('',*,*,#6832,.T.);
#9634=ORIENTED_EDGE('',*,*,#6833,.T.);
#9635=ORIENTED_EDGE('',*,*,#6834,.T.);
#9636=ORIENTED_EDGE('',*,*,#6835,.T.);
#9637=ORIENTED_EDGE('',*,*,#6836,.T.);
#9638=ORIENTED_EDGE('',*,*,#6837,.T.);
#9639=ORIENTED_EDGE('',*,*,#6838,.T.);
#9640=ORIENTED_EDGE('',*,*,#6825,.T.);
#9641=ORIENTED_EDGE('',*,*,#6838,.F.);
#9642=ORIENTED_EDGE('',*,*,#6839,.T.);
#9643=ORIENTED_EDGE('',*,*,#6840,.T.);
#9644=ORIENTED_EDGE('',*,*,#6841,.T.);
#9645=ORIENTED_EDGE('',*,*,#6842,.T.);
#9646=ORIENTED_EDGE('',*,*,#6843,.T.);
#9647=ORIENTED_EDGE('',*,*,#6844,.F.);
#9648=ORIENTED_EDGE('',*,*,#6845,.F.);
#9649=ORIENTED_EDGE('',*,*,#6846,.F.);
#9650=ORIENTED_EDGE('',*,*,#6847,.T.);
#9651=ORIENTED_EDGE('',*,*,#6847,.F.);
#9652=ORIENTED_EDGE('',*,*,#6848,.F.);
#9653=ORIENTED_EDGE('',*,*,#6849,.F.);
#9654=ORIENTED_EDGE('',*,*,#6850,.F.);
#9655=ORIENTED_EDGE('',*,*,#6851,.F.);
#9656=ORIENTED_EDGE('',*,*,#6851,.T.);
#9657=ORIENTED_EDGE('',*,*,#6828,.F.);
#9658=ORIENTED_EDGE('',*,*,#6852,.F.);
#9659=ORIENTED_EDGE('',*,*,#6853,.F.);
#9660=ORIENTED_EDGE('',*,*,#6854,.F.);
#9661=ORIENTED_EDGE('',*,*,#6816,.T.);
#9662=ORIENTED_EDGE('',*,*,#6855,.T.);
#9663=ORIENTED_EDGE('',*,*,#6856,.T.);
#9664=ORIENTED_EDGE('',*,*,#6857,.T.);
#9665=ORIENTED_EDGE('',*,*,#6858,.T.);
#9666=ORIENTED_EDGE('',*,*,#6859,.T.);
#9667=ORIENTED_EDGE('',*,*,#6860,.T.);
#9668=ORIENTED_EDGE('',*,*,#6861,.T.);
#9669=ORIENTED_EDGE('',*,*,#6862,.T.);
#9670=ORIENTED_EDGE('',*,*,#6863,.T.);
#9671=ORIENTED_EDGE('',*,*,#6864,.T.);
#9672=ORIENTED_EDGE('',*,*,#6853,.T.);
#9673=ORIENTED_EDGE('',*,*,#6865,.T.);
#9674=ORIENTED_EDGE('',*,*,#6866,.T.);
#9675=ORIENTED_EDGE('',*,*,#6867,.T.);
#9676=ORIENTED_EDGE('',*,*,#6868,.T.);
#9677=ORIENTED_EDGE('',*,*,#6869,.T.);
#9678=ORIENTED_EDGE('',*,*,#6855,.F.);
#9679=ORIENTED_EDGE('',*,*,#6852,.T.);
#9680=ORIENTED_EDGE('',*,*,#6843,.F.);
#9681=ORIENTED_EDGE('',*,*,#6870,.T.);
#9682=ORIENTED_EDGE('',*,*,#6865,.F.);
#9683=ORIENTED_EDGE('',*,*,#6848,.T.);
#9684=ORIENTED_EDGE('',*,*,#6846,.T.);
#9685=ORIENTED_EDGE('',*,*,#6871,.T.);
#9686=ORIENTED_EDGE('',*,*,#6872,.T.);
#9687=ORIENTED_EDGE('',*,*,#6873,.T.);
#9688=ORIENTED_EDGE('',*,*,#6874,.T.);
#9689=ORIENTED_EDGE('',*,*,#6875,.T.);
#9690=ORIENTED_EDGE('',*,*,#6876,.T.);
#9691=ORIENTED_EDGE('',*,*,#6877,.T.);
#9692=ORIENTED_EDGE('',*,*,#6878,.T.);
#9693=ORIENTED_EDGE('',*,*,#6879,.T.);
#9694=ORIENTED_EDGE('',*,*,#6878,.F.);
#9695=ORIENTED_EDGE('',*,*,#6880,.T.);
#9696=ORIENTED_EDGE('',*,*,#6881,.T.);
#9697=ORIENTED_EDGE('',*,*,#6882,.T.);
#9698=ORIENTED_EDGE('',*,*,#6883,.T.);
#9699=ORIENTED_EDGE('',*,*,#6884,.T.);
#9700=ORIENTED_EDGE('',*,*,#6885,.T.);
#9701=ORIENTED_EDGE('',*,*,#6886,.T.);
#9702=ORIENTED_EDGE('',*,*,#6887,.T.);
#9703=ORIENTED_EDGE('',*,*,#6888,.T.);
#9704=ORIENTED_EDGE('',*,*,#6889,.T.);
#9705=ORIENTED_EDGE('',*,*,#6890,.T.);
#9706=ORIENTED_EDGE('',*,*,#6891,.T.);
#9707=ORIENTED_EDGE('',*,*,#6892,.T.);
#9708=ORIENTED_EDGE('',*,*,#6845,.T.);
#9709=ORIENTED_EDGE('',*,*,#6893,.F.);
#9710=ORIENTED_EDGE('',*,*,#6894,.T.);
#9711=ORIENTED_EDGE('',*,*,#6871,.F.);
#9712=ORIENTED_EDGE('',*,*,#6895,.F.);
#9713=ORIENTED_EDGE('',*,*,#6896,.F.);
#9714=ORIENTED_EDGE('',*,*,#6873,.F.);
#9715=ORIENTED_EDGE('',*,*,#6897,.T.);
#9716=ORIENTED_EDGE('',*,*,#6897,.F.);
#9717=ORIENTED_EDGE('',*,*,#6872,.F.);
#9718=ORIENTED_EDGE('',*,*,#6894,.F.);
#9719=ORIENTED_EDGE('',*,*,#6898,.F.);
#9720=ORIENTED_EDGE('',*,*,#6899,.F.);
#9721=ORIENTED_EDGE('',*,*,#6899,.T.);
#9722=ORIENTED_EDGE('',*,*,#6842,.F.);
#9723=ORIENTED_EDGE('',*,*,#6900,.F.);
#9724=ORIENTED_EDGE('',*,*,#6866,.F.);
#9725=ORIENTED_EDGE('',*,*,#6870,.F.);
#9726=ORIENTED_EDGE('',*,*,#6900,.T.);
#9727=ORIENTED_EDGE('',*,*,#6841,.F.);
#9728=ORIENTED_EDGE('',*,*,#6901,.T.);
#9729=ORIENTED_EDGE('',*,*,#6867,.F.);
#9730=ORIENTED_EDGE('',*,*,#6896,.T.);
#9731=ORIENTED_EDGE('',*,*,#6902,.F.);
#9732=ORIENTED_EDGE('',*,*,#6903,.T.);
#9733=ORIENTED_EDGE('',*,*,#6874,.F.);
#9734=ORIENTED_EDGE('',*,*,#6904,.F.);
#9735=ORIENTED_EDGE('',*,*,#6905,.F.);
#9736=ORIENTED_EDGE('',*,*,#6876,.F.);
#9737=ORIENTED_EDGE('',*,*,#6906,.T.);
#9738=ORIENTED_EDGE('',*,*,#6906,.F.);
#9739=ORIENTED_EDGE('',*,*,#6875,.F.);
#9740=ORIENTED_EDGE('',*,*,#6903,.F.);
#9741=ORIENTED_EDGE('',*,*,#6907,.F.);
#9742=ORIENTED_EDGE('',*,*,#6908,.F.);
#9743=ORIENTED_EDGE('',*,*,#6908,.T.);
#9744=ORIENTED_EDGE('',*,*,#6840,.F.);
#9745=ORIENTED_EDGE('',*,*,#6909,.F.);
#9746=ORIENTED_EDGE('',*,*,#6868,.F.);
#9747=ORIENTED_EDGE('',*,*,#6901,.F.);
#9748=ORIENTED_EDGE('',*,*,#6909,.T.);
#9749=ORIENTED_EDGE('',*,*,#6839,.F.);
#9750=ORIENTED_EDGE('',*,*,#6837,.F.);
#9751=ORIENTED_EDGE('',*,*,#6910,.T.);
#9752=ORIENTED_EDGE('',*,*,#6856,.F.);
#9753=ORIENTED_EDGE('',*,*,#6869,.F.);
#9754=ORIENTED_EDGE('',*,*,#6905,.T.);
#9755=ORIENTED_EDGE('',*,*,#6911,.F.);
#9756=ORIENTED_EDGE('',*,*,#6912,.F.);
#9757=ORIENTED_EDGE('',*,*,#6913,.T.);
#9758=ORIENTED_EDGE('',*,*,#6880,.F.);
#9759=ORIENTED_EDGE('',*,*,#6877,.F.);
#9760=ORIENTED_EDGE('',*,*,#6914,.F.);
#9761=ORIENTED_EDGE('',*,*,#6915,.F.);
#9762=ORIENTED_EDGE('',*,*,#6882,.F.);
#9763=ORIENTED_EDGE('',*,*,#6916,.T.);
#9764=ORIENTED_EDGE('',*,*,#6916,.F.);
#9765=ORIENTED_EDGE('',*,*,#6881,.F.);
#9766=ORIENTED_EDGE('',*,*,#6913,.F.);
#9767=ORIENTED_EDGE('',*,*,#6917,.F.);
#9768=ORIENTED_EDGE('',*,*,#6918,.F.);
#9769=ORIENTED_EDGE('',*,*,#6918,.T.);
#9770=ORIENTED_EDGE('',*,*,#6836,.F.);
#9771=ORIENTED_EDGE('',*,*,#6919,.F.);
#9772=ORIENTED_EDGE('',*,*,#6857,.F.);
#9773=ORIENTED_EDGE('',*,*,#6910,.F.);
#9774=ORIENTED_EDGE('',*,*,#6919,.T.);
#9775=ORIENTED_EDGE('',*,*,#6835,.F.);
#9776=ORIENTED_EDGE('',*,*,#6920,.T.);
#9777=ORIENTED_EDGE('',*,*,#6858,.F.);
#9778=ORIENTED_EDGE('',*,*,#6915,.T.);
#9779=ORIENTED_EDGE('',*,*,#6921,.F.);
#9780=ORIENTED_EDGE('',*,*,#6922,.T.);
#9781=ORIENTED_EDGE('',*,*,#6883,.F.);
#9782=ORIENTED_EDGE('',*,*,#6923,.F.);
#9783=ORIENTED_EDGE('',*,*,#6924,.F.);
#9784=ORIENTED_EDGE('',*,*,#6885,.F.);
#9785=ORIENTED_EDGE('',*,*,#6925,.T.);
#9786=ORIENTED_EDGE('',*,*,#6925,.F.);
#9787=ORIENTED_EDGE('',*,*,#6884,.F.);
#9788=ORIENTED_EDGE('',*,*,#6922,.F.);
#9789=ORIENTED_EDGE('',*,*,#6926,.F.);
#9790=ORIENTED_EDGE('',*,*,#6927,.F.);
#9791=ORIENTED_EDGE('',*,*,#6927,.T.);
#9792=ORIENTED_EDGE('',*,*,#6834,.F.);
#9793=ORIENTED_EDGE('',*,*,#6928,.F.);
#9794=ORIENTED_EDGE('',*,*,#6859,.F.);
#9795=ORIENTED_EDGE('',*,*,#6920,.F.);
#9796=ORIENTED_EDGE('',*,*,#6928,.T.);
#9797=ORIENTED_EDGE('',*,*,#6833,.F.);
#9798=ORIENTED_EDGE('',*,*,#6929,.T.);
#9799=ORIENTED_EDGE('',*,*,#6860,.F.);
#9800=ORIENTED_EDGE('',*,*,#6924,.T.);
#9801=ORIENTED_EDGE('',*,*,#6930,.F.);
#9802=ORIENTED_EDGE('',*,*,#6931,.T.);
#9803=ORIENTED_EDGE('',*,*,#6886,.F.);
#9804=ORIENTED_EDGE('',*,*,#6887,.F.);
#9805=ORIENTED_EDGE('',*,*,#6931,.F.);
#9806=ORIENTED_EDGE('',*,*,#6932,.F.);
#9807=ORIENTED_EDGE('',*,*,#6933,.F.);
#9808=ORIENTED_EDGE('',*,*,#6933,.T.);
#9809=ORIENTED_EDGE('',*,*,#6934,.F.);
#9810=ORIENTED_EDGE('',*,*,#6935,.F.);
#9811=ORIENTED_EDGE('',*,*,#6888,.F.);
#9812=ORIENTED_EDGE('',*,*,#6936,.T.);
#9813=ORIENTED_EDGE('',*,*,#6936,.F.);
#9814=ORIENTED_EDGE('',*,*,#6861,.F.);
#9815=ORIENTED_EDGE('',*,*,#6929,.F.);
#9816=ORIENTED_EDGE('',*,*,#6832,.F.);
#9817=ORIENTED_EDGE('',*,*,#6937,.F.);
#9818=ORIENTED_EDGE('',*,*,#6823,.T.);
#9819=ORIENTED_EDGE('',*,*,#6938,.T.);
#9820=ORIENTED_EDGE('',*,*,#6939,.F.);
#9821=ORIENTED_EDGE('',*,*,#6938,.F.);
#9822=ORIENTED_EDGE('',*,*,#6854,.T.);
#9823=ORIENTED_EDGE('',*,*,#6864,.F.);
#9824=ORIENTED_EDGE('',*,*,#6940,.T.);
#9825=ORIENTED_EDGE('',*,*,#6829,.F.);
#9826=ORIENTED_EDGE('',*,*,#6941,.F.);
#9827=ORIENTED_EDGE('',*,*,#6942,.T.);
#9828=ORIENTED_EDGE('',*,*,#6911,.T.);
#9829=ORIENTED_EDGE('',*,*,#6904,.T.);
#9830=ORIENTED_EDGE('',*,*,#6907,.T.);
#9831=ORIENTED_EDGE('',*,*,#6902,.T.);
#9832=ORIENTED_EDGE('',*,*,#6895,.T.);
#9833=ORIENTED_EDGE('',*,*,#6898,.T.);
#9834=ORIENTED_EDGE('',*,*,#6893,.T.);
#9835=ORIENTED_EDGE('',*,*,#6844,.T.);
#9836=ORIENTED_EDGE('',*,*,#6850,.T.);
#9837=ORIENTED_EDGE('',*,*,#6943,.T.);
#9838=ORIENTED_EDGE('',*,*,#6944,.T.);
#9839=ORIENTED_EDGE('',*,*,#6945,.T.);
#9840=ORIENTED_EDGE('',*,*,#6946,.T.);
#9841=ORIENTED_EDGE('',*,*,#6934,.T.);
#9842=ORIENTED_EDGE('',*,*,#6932,.T.);
#9843=ORIENTED_EDGE('',*,*,#6930,.T.);
#9844=ORIENTED_EDGE('',*,*,#6923,.T.);
#9845=ORIENTED_EDGE('',*,*,#6926,.T.);
#9846=ORIENTED_EDGE('',*,*,#6921,.T.);
#9847=ORIENTED_EDGE('',*,*,#6914,.T.);
#9848=ORIENTED_EDGE('',*,*,#6917,.T.);
#9849=ORIENTED_EDGE('',*,*,#6912,.T.);
#9850=ORIENTED_EDGE('',*,*,#6942,.F.);
#9851=ORIENTED_EDGE('',*,*,#6849,.T.);
#9852=ORIENTED_EDGE('',*,*,#6892,.F.);
#9853=ORIENTED_EDGE('',*,*,#6947,.T.);
#9854=ORIENTED_EDGE('',*,*,#6943,.F.);
#9855=ORIENTED_EDGE('',*,*,#6947,.F.);
#9856=ORIENTED_EDGE('',*,*,#6891,.F.);
#9857=ORIENTED_EDGE('',*,*,#6948,.T.);
#9858=ORIENTED_EDGE('',*,*,#6948,.F.);
#9859=ORIENTED_EDGE('',*,*,#6890,.F.);
#9860=ORIENTED_EDGE('',*,*,#6949,.F.);
#9861=ORIENTED_EDGE('',*,*,#6945,.F.);
#9862=ORIENTED_EDGE('',*,*,#6950,.F.);
#9863=ORIENTED_EDGE('',*,*,#6950,.T.);
#9864=ORIENTED_EDGE('',*,*,#6944,.F.);
#9865=ORIENTED_EDGE('',*,*,#6940,.F.);
#9866=ORIENTED_EDGE('',*,*,#6863,.F.);
#9867=ORIENTED_EDGE('',*,*,#6951,.F.);
#9868=ORIENTED_EDGE('',*,*,#6830,.F.);
#9869=ORIENTED_EDGE('',*,*,#6937,.T.);
#9870=ORIENTED_EDGE('',*,*,#6831,.F.);
#9871=ORIENTED_EDGE('',*,*,#6951,.T.);
#9872=ORIENTED_EDGE('',*,*,#6862,.F.);
#9873=ORIENTED_EDGE('',*,*,#6952,.F.);
#9874=ORIENTED_EDGE('',*,*,#6939,.T.);
#9875=ORIENTED_EDGE('',*,*,#6953,.F.);
#9876=ORIENTED_EDGE('',*,*,#6954,.T.);
#9877=ORIENTED_EDGE('',*,*,#6952,.T.);
#9878=ORIENTED_EDGE('',*,*,#6954,.F.);
#9879=ORIENTED_EDGE('',*,*,#6955,.F.);
#9880=ORIENTED_EDGE('',*,*,#6956,.T.);
#9881=ORIENTED_EDGE('',*,*,#6953,.T.);
#9882=ORIENTED_EDGE('',*,*,#6956,.F.);
#9883=ORIENTED_EDGE('',*,*,#6957,.F.);
#9884=ORIENTED_EDGE('',*,*,#6958,.T.);
#9885=ORIENTED_EDGE('',*,*,#6955,.T.);
#9886=ORIENTED_EDGE('',*,*,#6958,.F.);
#9887=ORIENTED_EDGE('',*,*,#6957,.T.);
#9888=ORIENTED_EDGE('',*,*,#6821,.F.);
#9889=ORIENTED_EDGE('',*,*,#6935,.T.);
#9890=ORIENTED_EDGE('',*,*,#6946,.F.);
#9891=ORIENTED_EDGE('',*,*,#6949,.T.);
#9892=ORIENTED_EDGE('',*,*,#6889,.F.);
#9893=ORIENTED_EDGE('',*,*,#6959,.T.);
#9894=ORIENTED_EDGE('',*,*,#6960,.T.);
#9895=ORIENTED_EDGE('',*,*,#6961,.F.);
#9896=ORIENTED_EDGE('',*,*,#6960,.F.);
#9897=ORIENTED_EDGE('',*,*,#6961,.T.);
#9898=ORIENTED_EDGE('',*,*,#6962,.T.);
#9899=ORIENTED_EDGE('',*,*,#6963,.F.);
#9900=ORIENTED_EDGE('',*,*,#6962,.F.);
#9901=ORIENTED_EDGE('',*,*,#6879,.F.);
#9902=ORIENTED_EDGE('',*,*,#6963,.T.);
#9903=ORIENTED_EDGE('',*,*,#6941,.T.);
#9904=ORIENTED_EDGE('',*,*,#6964,.F.);
#9905=ORIENTED_EDGE('',*,*,#6964,.T.);
#9906=ORIENTED_EDGE('',*,*,#6965,.T.);
#9907=ORIENTED_EDGE('',*,*,#6959,.F.);
#9908=ORIENTED_EDGE('',*,*,#6965,.F.);
#9909=ORIENTED_EDGE('',*,*,#6966,.T.);
#9910=ORIENTED_EDGE('',*,*,#6967,.T.);
#9911=ORIENTED_EDGE('',*,*,#6968,.F.);
#9912=ORIENTED_EDGE('',*,*,#6967,.F.);
#9913=ORIENTED_EDGE('',*,*,#6969,.F.);
#9914=ORIENTED_EDGE('',*,*,#6968,.T.);
#9915=ORIENTED_EDGE('',*,*,#6970,.F.);
#9916=ORIENTED_EDGE('',*,*,#6971,.T.);
#9917=ORIENTED_EDGE('',*,*,#6969,.T.);
#9918=ORIENTED_EDGE('',*,*,#6971,.F.);
#9919=ORIENTED_EDGE('',*,*,#6970,.T.);
#9920=ORIENTED_EDGE('',*,*,#6966,.F.);
#9921=ORIENTED_EDGE('',*,*,#6972,.T.);
#9922=ORIENTED_EDGE('',*,*,#6973,.T.);
#9923=ORIENTED_EDGE('',*,*,#6974,.T.);
#9924=ORIENTED_EDGE('',*,*,#6975,.T.);
#9925=ORIENTED_EDGE('',*,*,#6973,.F.);
#9926=ORIENTED_EDGE('',*,*,#6976,.T.);
#9927=ORIENTED_EDGE('',*,*,#6977,.F.);
#9928=ORIENTED_EDGE('',*,*,#6978,.F.);
#9929=ORIENTED_EDGE('',*,*,#6972,.F.);
#9930=ORIENTED_EDGE('',*,*,#6979,.T.);
#9931=ORIENTED_EDGE('',*,*,#6980,.T.);
#9932=ORIENTED_EDGE('',*,*,#6981,.F.);
#9933=ORIENTED_EDGE('',*,*,#6982,.F.);
#9934=ORIENTED_EDGE('',*,*,#6976,.F.);
#9935=ORIENTED_EDGE('',*,*,#6983,.T.);
#9936=ORIENTED_EDGE('',*,*,#6984,.T.);
#9937=ORIENTED_EDGE('',*,*,#6985,.T.);
#9938=ORIENTED_EDGE('',*,*,#6986,.T.);
#9939=ORIENTED_EDGE('',*,*,#6986,.F.);
#9940=ORIENTED_EDGE('',*,*,#6987,.F.);
#9941=ORIENTED_EDGE('',*,*,#6988,.F.);
#9942=ORIENTED_EDGE('',*,*,#6989,.F.);
#9943=ORIENTED_EDGE('',*,*,#6974,.F.);
#9944=ORIENTED_EDGE('',*,*,#6978,.T.);
#9945=ORIENTED_EDGE('',*,*,#6990,.F.);
#9946=ORIENTED_EDGE('',*,*,#6991,.F.);
#9947=ORIENTED_EDGE('',*,*,#6992,.F.);
#9948=ORIENTED_EDGE('',*,*,#6987,.T.);
#9949=ORIENTED_EDGE('',*,*,#6985,.F.);
#9950=ORIENTED_EDGE('',*,*,#6993,.T.);
#9951=ORIENTED_EDGE('',*,*,#6982,.T.);
#9952=ORIENTED_EDGE('',*,*,#6994,.T.);
#9953=ORIENTED_EDGE('',*,*,#6990,.T.);
#9954=ORIENTED_EDGE('',*,*,#6977,.T.);
#9955=ORIENTED_EDGE('',*,*,#6994,.F.);
#9956=ORIENTED_EDGE('',*,*,#6981,.T.);
#9957=ORIENTED_EDGE('',*,*,#6995,.T.);
#9958=ORIENTED_EDGE('',*,*,#6996,.T.);
#9959=ORIENTED_EDGE('',*,*,#6997,.T.);
#9960=ORIENTED_EDGE('',*,*,#6998,.T.);
#9961=ORIENTED_EDGE('',*,*,#6999,.T.);
#9962=ORIENTED_EDGE('',*,*,#7000,.T.);
#9963=ORIENTED_EDGE('',*,*,#7001,.F.);
#9964=ORIENTED_EDGE('',*,*,#6991,.T.);
#9965=ORIENTED_EDGE('',*,*,#7002,.T.);
#9966=ORIENTED_EDGE('',*,*,#7003,.T.);
#9967=ORIENTED_EDGE('',*,*,#7004,.T.);
#9968=ORIENTED_EDGE('',*,*,#6988,.T.);
#9969=ORIENTED_EDGE('',*,*,#6992,.T.);
#9970=ORIENTED_EDGE('',*,*,#7001,.T.);
#9971=ORIENTED_EDGE('',*,*,#6983,.F.);
#9972=ORIENTED_EDGE('',*,*,#6989,.T.);
#9973=ORIENTED_EDGE('',*,*,#7004,.F.);
#9974=ORIENTED_EDGE('',*,*,#7000,.F.);
#9975=ORIENTED_EDGE('',*,*,#7005,.F.);
#9976=ORIENTED_EDGE('',*,*,#7006,.F.);
#9977=ORIENTED_EDGE('',*,*,#7007,.F.);
#9978=ORIENTED_EDGE('',*,*,#7008,.T.);
#9979=ORIENTED_EDGE('',*,*,#7003,.F.);
#9980=ORIENTED_EDGE('',*,*,#7008,.F.);
#9981=ORIENTED_EDGE('',*,*,#7009,.F.);
#9982=ORIENTED_EDGE('',*,*,#7010,.T.);
#9983=ORIENTED_EDGE('',*,*,#7002,.F.);
#9984=ORIENTED_EDGE('',*,*,#7010,.F.);
#9985=ORIENTED_EDGE('',*,*,#7011,.F.);
#9986=ORIENTED_EDGE('',*,*,#7012,.F.);
#9987=ORIENTED_EDGE('',*,*,#7013,.T.);
#9988=ORIENTED_EDGE('',*,*,#6998,.F.);
#9989=ORIENTED_EDGE('',*,*,#7014,.F.);
#9990=ORIENTED_EDGE('',*,*,#7005,.T.);
#9991=ORIENTED_EDGE('',*,*,#6999,.F.);
#9992=ORIENTED_EDGE('',*,*,#7013,.F.);
#9993=ORIENTED_EDGE('',*,*,#7015,.F.);
#9994=ORIENTED_EDGE('',*,*,#6996,.F.);
#9995=ORIENTED_EDGE('',*,*,#7016,.F.);
#9996=ORIENTED_EDGE('',*,*,#7017,.T.);
#9997=ORIENTED_EDGE('',*,*,#7018,.T.);
#9998=ORIENTED_EDGE('',*,*,#7016,.T.);
#9999=ORIENTED_EDGE('',*,*,#6995,.F.);
#10000=ORIENTED_EDGE('',*,*,#6980,.F.);
#10001=ORIENTED_EDGE('',*,*,#6975,.F.);
#10002=ORIENTED_EDGE('',*,*,#6993,.F.);
#10003=ORIENTED_EDGE('',*,*,#6984,.F.);
#10004=ORIENTED_EDGE('',*,*,#7006,.T.);
#10005=ORIENTED_EDGE('',*,*,#7014,.T.);
#10006=ORIENTED_EDGE('',*,*,#7012,.T.);
#10007=ORIENTED_EDGE('',*,*,#7019,.F.);
#10008=ORIENTED_EDGE('',*,*,#7017,.F.);
#10009=ORIENTED_EDGE('',*,*,#7018,.F.);
#10010=ORIENTED_EDGE('',*,*,#6979,.F.);
#10011=ORIENTED_EDGE('',*,*,#7007,.T.);
#10012=ORIENTED_EDGE('',*,*,#7009,.T.);
#10013=ORIENTED_EDGE('',*,*,#7011,.T.);
#10014=ORIENTED_EDGE('',*,*,#6997,.F.);
#10015=ORIENTED_EDGE('',*,*,#7015,.T.);
#10016=ORIENTED_EDGE('',*,*,#7019,.T.);
#10017=ORIENTED_EDGE('',*,*,#7020,.F.);
#10018=ORIENTED_EDGE('',*,*,#7021,.T.);
#10019=ORIENTED_EDGE('',*,*,#7022,.T.);
#10020=ORIENTED_EDGE('',*,*,#7023,.T.);
#10021=ORIENTED_EDGE('',*,*,#7024,.F.);
#10022=ORIENTED_EDGE('',*,*,#7025,.T.);
#10023=ORIENTED_EDGE('',*,*,#7020,.T.);
#10024=ORIENTED_EDGE('',*,*,#7026,.T.);
#10025=ORIENTED_EDGE('',*,*,#7027,.F.);
#10026=ORIENTED_EDGE('',*,*,#7028,.T.);
#10027=ORIENTED_EDGE('',*,*,#7024,.T.);
#10028=ORIENTED_EDGE('',*,*,#7029,.T.);
#10029=ORIENTED_EDGE('',*,*,#7030,.F.);
#10030=ORIENTED_EDGE('',*,*,#7031,.T.);
#10031=ORIENTED_EDGE('',*,*,#7027,.T.);
#10032=ORIENTED_EDGE('',*,*,#7032,.T.);
#10033=ORIENTED_EDGE('',*,*,#7033,.F.);
#10034=ORIENTED_EDGE('',*,*,#7034,.T.);
#10035=ORIENTED_EDGE('',*,*,#7030,.T.);
#10036=ORIENTED_EDGE('',*,*,#7035,.T.);
#10037=ORIENTED_EDGE('',*,*,#7036,.F.);
#10038=ORIENTED_EDGE('',*,*,#7037,.T.);
#10039=ORIENTED_EDGE('',*,*,#7033,.T.);
#10040=ORIENTED_EDGE('',*,*,#7038,.T.);
#10041=ORIENTED_EDGE('',*,*,#7039,.F.);
#10042=ORIENTED_EDGE('',*,*,#7040,.T.);
#10043=ORIENTED_EDGE('',*,*,#7041,.F.);
#10044=ORIENTED_EDGE('',*,*,#7042,.F.);
#10045=ORIENTED_EDGE('',*,*,#7043,.T.);
#10046=ORIENTED_EDGE('',*,*,#7039,.T.);
#10047=ORIENTED_EDGE('',*,*,#7044,.F.);
#10048=ORIENTED_EDGE('',*,*,#7045,.F.);
#10049=ORIENTED_EDGE('',*,*,#7046,.F.);
#10050=ORIENTED_EDGE('',*,*,#7047,.T.);
#10051=ORIENTED_EDGE('',*,*,#7042,.T.);
#10052=ORIENTED_EDGE('',*,*,#7048,.F.);
#10053=ORIENTED_EDGE('',*,*,#7049,.F.);
#10054=ORIENTED_EDGE('',*,*,#7050,.T.);
#10055=ORIENTED_EDGE('',*,*,#7046,.T.);
#10056=ORIENTED_EDGE('',*,*,#7051,.F.);
#10057=ORIENTED_EDGE('',*,*,#7052,.F.);
#10058=ORIENTED_EDGE('',*,*,#7053,.T.);
#10059=ORIENTED_EDGE('',*,*,#7049,.T.);
#10060=ORIENTED_EDGE('',*,*,#7054,.F.);
#10061=ORIENTED_EDGE('',*,*,#7055,.F.);
#10062=ORIENTED_EDGE('',*,*,#7056,.T.);
#10063=ORIENTED_EDGE('',*,*,#7052,.T.);
#10064=ORIENTED_EDGE('',*,*,#7057,.F.);
#10065=ORIENTED_EDGE('',*,*,#7044,.T.);
#10066=ORIENTED_EDGE('',*,*,#7041,.T.);
#10067=ORIENTED_EDGE('',*,*,#7058,.T.);
#10068=ORIENTED_EDGE('',*,*,#7059,.F.);
#10069=ORIENTED_EDGE('',*,*,#7060,.F.);
#10070=ORIENTED_EDGE('',*,*,#7061,.T.);
#10071=ORIENTED_EDGE('',*,*,#7061,.F.);
#10072=ORIENTED_EDGE('',*,*,#7062,.F.);
#10073=ORIENTED_EDGE('',*,*,#7038,.F.);
#10074=ORIENTED_EDGE('',*,*,#7035,.F.);
#10075=ORIENTED_EDGE('',*,*,#7032,.F.);
#10076=ORIENTED_EDGE('',*,*,#7029,.F.);
#10077=ORIENTED_EDGE('',*,*,#7026,.F.);
#10078=ORIENTED_EDGE('',*,*,#7023,.F.);
#10079=ORIENTED_EDGE('',*,*,#7063,.F.);
#10080=ORIENTED_EDGE('',*,*,#7064,.T.);
#10081=ORIENTED_EDGE('',*,*,#7057,.T.);
#10082=ORIENTED_EDGE('',*,*,#7054,.T.);
#10083=ORIENTED_EDGE('',*,*,#7051,.T.);
#10084=ORIENTED_EDGE('',*,*,#7048,.T.);
#10085=ORIENTED_EDGE('',*,*,#7045,.T.);
#10086=ORIENTED_EDGE('',*,*,#7065,.T.);
#10087=ORIENTED_EDGE('',*,*,#7066,.T.);
#10088=ORIENTED_EDGE('',*,*,#7067,.T.);
#10089=ORIENTED_EDGE('',*,*,#7068,.T.);
#10090=ORIENTED_EDGE('',*,*,#7063,.T.);
#10091=ORIENTED_EDGE('',*,*,#7055,.T.);
#10092=ORIENTED_EDGE('',*,*,#7064,.F.);
#10093=ORIENTED_EDGE('',*,*,#7068,.F.);
#10094=ORIENTED_EDGE('',*,*,#7069,.T.);
#10095=ORIENTED_EDGE('',*,*,#7058,.F.);
#10096=ORIENTED_EDGE('',*,*,#7040,.F.);
#10097=ORIENTED_EDGE('',*,*,#7043,.F.);
#10098=ORIENTED_EDGE('',*,*,#7047,.F.);
#10099=ORIENTED_EDGE('',*,*,#7050,.F.);
#10100=ORIENTED_EDGE('',*,*,#7053,.F.);
#10101=ORIENTED_EDGE('',*,*,#7056,.F.);
#10102=ORIENTED_EDGE('',*,*,#7069,.F.);
#10103=ORIENTED_EDGE('',*,*,#7067,.F.);
#10104=ORIENTED_EDGE('',*,*,#7021,.F.);
#10105=ORIENTED_EDGE('',*,*,#7025,.F.);
#10106=ORIENTED_EDGE('',*,*,#7028,.F.);
#10107=ORIENTED_EDGE('',*,*,#7031,.F.);
#10108=ORIENTED_EDGE('',*,*,#7034,.F.);
#10109=ORIENTED_EDGE('',*,*,#7037,.F.);
#10110=ORIENTED_EDGE('',*,*,#7070,.F.);
#10111=ORIENTED_EDGE('',*,*,#7071,.F.);
#10112=ORIENTED_EDGE('',*,*,#7072,.T.);
#10113=ORIENTED_EDGE('',*,*,#7073,.T.);
#10114=ORIENTED_EDGE('',*,*,#7074,.F.);
#10115=ORIENTED_EDGE('',*,*,#7075,.F.);
#10116=ORIENTED_EDGE('',*,*,#7076,.T.);
#10117=ORIENTED_EDGE('',*,*,#7077,.T.);
#10118=ORIENTED_EDGE('',*,*,#7072,.F.);
#10119=ORIENTED_EDGE('',*,*,#7078,.F.);
#10120=ORIENTED_EDGE('',*,*,#7079,.T.);
#10121=ORIENTED_EDGE('',*,*,#7080,.T.);
#10122=ORIENTED_EDGE('',*,*,#7076,.F.);
#10123=ORIENTED_EDGE('',*,*,#7081,.F.);
#10124=ORIENTED_EDGE('',*,*,#7082,.T.);
#10125=ORIENTED_EDGE('',*,*,#7083,.T.);
#10126=ORIENTED_EDGE('',*,*,#7079,.F.);
#10127=ORIENTED_EDGE('',*,*,#7084,.F.);
#10128=ORIENTED_EDGE('',*,*,#7085,.T.);
#10129=ORIENTED_EDGE('',*,*,#7086,.T.);
#10130=ORIENTED_EDGE('',*,*,#7082,.F.);
#10131=ORIENTED_EDGE('',*,*,#7087,.F.);
#10132=ORIENTED_EDGE('',*,*,#7074,.T.);
#10133=ORIENTED_EDGE('',*,*,#7088,.T.);
#10134=ORIENTED_EDGE('',*,*,#7085,.F.);
#10135=ORIENTED_EDGE('',*,*,#7088,.F.);
#10136=ORIENTED_EDGE('',*,*,#7073,.F.);
#10137=ORIENTED_EDGE('',*,*,#7077,.F.);
#10138=ORIENTED_EDGE('',*,*,#7080,.F.);
#10139=ORIENTED_EDGE('',*,*,#7083,.F.);
#10140=ORIENTED_EDGE('',*,*,#7086,.F.);
#10141=ORIENTED_EDGE('',*,*,#7089,.F.);
#10142=ORIENTED_EDGE('',*,*,#7071,.T.);
#10143=ORIENTED_EDGE('',*,*,#7087,.T.);
#10144=ORIENTED_EDGE('',*,*,#7084,.T.);
#10145=ORIENTED_EDGE('',*,*,#7081,.T.);
#10146=ORIENTED_EDGE('',*,*,#7078,.T.);
#10147=ORIENTED_EDGE('',*,*,#7075,.T.);
#10148=ORIENTED_EDGE('',*,*,#7065,.F.);
#10149=ORIENTED_EDGE('',*,*,#7022,.F.);
#10150=ORIENTED_EDGE('',*,*,#7066,.F.);
#10151=ORIENTED_EDGE('',*,*,#7090,.T.);
#10152=ORIENTED_EDGE('',*,*,#7089,.T.);
#10153=ORIENTED_EDGE('',*,*,#7090,.F.);
#10154=ORIENTED_EDGE('',*,*,#7036,.T.);
#10155=ORIENTED_EDGE('',*,*,#7062,.T.);
#10156=ORIENTED_EDGE('',*,*,#7091,.F.);
#10157=ORIENTED_EDGE('',*,*,#7070,.T.);
#10158=ORIENTED_EDGE('',*,*,#7092,.F.);
#10159=ORIENTED_EDGE('',*,*,#7093,.T.);
#10160=ORIENTED_EDGE('',*,*,#7059,.T.);
#10161=ORIENTED_EDGE('',*,*,#7091,.T.);
#10162=ORIENTED_EDGE('',*,*,#7060,.T.);
#10163=ORIENTED_EDGE('',*,*,#7093,.F.);
#10164=ORIENTED_EDGE('',*,*,#7092,.T.);
#10165=ORIENTED_EDGE('',*,*,#7094,.F.);
#10166=ORIENTED_EDGE('',*,*,#7095,.T.);
#10167=ORIENTED_EDGE('',*,*,#7096,.T.);
#10168=ORIENTED_EDGE('',*,*,#7097,.T.);
#10169=ORIENTED_EDGE('',*,*,#7098,.F.);
#10170=ORIENTED_EDGE('',*,*,#7099,.T.);
#10171=ORIENTED_EDGE('',*,*,#7094,.T.);
#10172=ORIENTED_EDGE('',*,*,#7100,.T.);
#10173=ORIENTED_EDGE('',*,*,#7101,.F.);
#10174=ORIENTED_EDGE('',*,*,#7102,.T.);
#10175=ORIENTED_EDGE('',*,*,#7098,.T.);
#10176=ORIENTED_EDGE('',*,*,#7103,.T.);
#10177=ORIENTED_EDGE('',*,*,#7104,.F.);
#10178=ORIENTED_EDGE('',*,*,#7105,.T.);
#10179=ORIENTED_EDGE('',*,*,#7101,.T.);
#10180=ORIENTED_EDGE('',*,*,#7106,.T.);
#10181=ORIENTED_EDGE('',*,*,#7107,.F.);
#10182=ORIENTED_EDGE('',*,*,#7108,.T.);
#10183=ORIENTED_EDGE('',*,*,#7104,.T.);
#10184=ORIENTED_EDGE('',*,*,#7109,.T.);
#10185=ORIENTED_EDGE('',*,*,#7110,.F.);
#10186=ORIENTED_EDGE('',*,*,#7111,.T.);
#10187=ORIENTED_EDGE('',*,*,#7107,.T.);
#10188=ORIENTED_EDGE('',*,*,#7112,.T.);
#10189=ORIENTED_EDGE('',*,*,#7113,.F.);
#10190=ORIENTED_EDGE('',*,*,#7114,.T.);
#10191=ORIENTED_EDGE('',*,*,#7110,.T.);
#10192=ORIENTED_EDGE('',*,*,#7115,.T.);
#10193=ORIENTED_EDGE('',*,*,#7116,.F.);
#10194=ORIENTED_EDGE('',*,*,#7117,.T.);
#10195=ORIENTED_EDGE('',*,*,#7113,.T.);
#10196=ORIENTED_EDGE('',*,*,#7118,.T.);
#10197=ORIENTED_EDGE('',*,*,#7119,.F.);
#10198=ORIENTED_EDGE('',*,*,#7120,.T.);
#10199=ORIENTED_EDGE('',*,*,#7116,.T.);
#10200=ORIENTED_EDGE('',*,*,#7121,.T.);
#10201=ORIENTED_EDGE('',*,*,#7122,.F.);
#10202=ORIENTED_EDGE('',*,*,#7123,.T.);
#10203=ORIENTED_EDGE('',*,*,#7119,.T.);
#10204=ORIENTED_EDGE('',*,*,#7124,.T.);
#10205=ORIENTED_EDGE('',*,*,#7125,.F.);
#10206=ORIENTED_EDGE('',*,*,#7126,.T.);
#10207=ORIENTED_EDGE('',*,*,#7122,.T.);
#10208=ORIENTED_EDGE('',*,*,#7127,.T.);
#10209=ORIENTED_EDGE('',*,*,#7128,.F.);
#10210=ORIENTED_EDGE('',*,*,#7129,.T.);
#10211=ORIENTED_EDGE('',*,*,#7125,.T.);
#10212=ORIENTED_EDGE('',*,*,#7130,.T.);
#10213=ORIENTED_EDGE('',*,*,#7131,.F.);
#10214=ORIENTED_EDGE('',*,*,#7132,.T.);
#10215=ORIENTED_EDGE('',*,*,#7128,.T.);
#10216=ORIENTED_EDGE('',*,*,#7133,.T.);
#10217=ORIENTED_EDGE('',*,*,#7134,.F.);
#10218=ORIENTED_EDGE('',*,*,#7135,.T.);
#10219=ORIENTED_EDGE('',*,*,#7131,.T.);
#10220=ORIENTED_EDGE('',*,*,#7136,.T.);
#10221=ORIENTED_EDGE('',*,*,#7137,.F.);
#10222=ORIENTED_EDGE('',*,*,#7138,.T.);
#10223=ORIENTED_EDGE('',*,*,#7134,.T.);
#10224=ORIENTED_EDGE('',*,*,#7139,.T.);
#10225=ORIENTED_EDGE('',*,*,#7140,.F.);
#10226=ORIENTED_EDGE('',*,*,#7141,.T.);
#10227=ORIENTED_EDGE('',*,*,#7137,.T.);
#10228=ORIENTED_EDGE('',*,*,#7142,.T.);
#10229=ORIENTED_EDGE('',*,*,#7143,.F.);
#10230=ORIENTED_EDGE('',*,*,#7144,.T.);
#10231=ORIENTED_EDGE('',*,*,#7140,.T.);
#10232=ORIENTED_EDGE('',*,*,#7145,.T.);
#10233=ORIENTED_EDGE('',*,*,#7146,.F.);
#10234=ORIENTED_EDGE('',*,*,#7147,.T.);
#10235=ORIENTED_EDGE('',*,*,#7143,.T.);
#10236=ORIENTED_EDGE('',*,*,#7148,.T.);
#10237=ORIENTED_EDGE('',*,*,#7149,.F.);
#10238=ORIENTED_EDGE('',*,*,#7150,.T.);
#10239=ORIENTED_EDGE('',*,*,#7146,.T.);
#10240=ORIENTED_EDGE('',*,*,#7151,.T.);
#10241=ORIENTED_EDGE('',*,*,#7152,.F.);
#10242=ORIENTED_EDGE('',*,*,#7153,.T.);
#10243=ORIENTED_EDGE('',*,*,#7149,.T.);
#10244=ORIENTED_EDGE('',*,*,#7154,.T.);
#10245=ORIENTED_EDGE('',*,*,#7155,.F.);
#10246=ORIENTED_EDGE('',*,*,#7156,.T.);
#10247=ORIENTED_EDGE('',*,*,#7152,.T.);
#10248=ORIENTED_EDGE('',*,*,#7157,.T.);
#10249=ORIENTED_EDGE('',*,*,#7158,.F.);
#10250=ORIENTED_EDGE('',*,*,#7159,.T.);
#10251=ORIENTED_EDGE('',*,*,#7155,.T.);
#10252=ORIENTED_EDGE('',*,*,#7160,.T.);
#10253=ORIENTED_EDGE('',*,*,#7161,.F.);
#10254=ORIENTED_EDGE('',*,*,#7162,.T.);
#10255=ORIENTED_EDGE('',*,*,#7158,.T.);
#10256=ORIENTED_EDGE('',*,*,#7163,.T.);
#10257=ORIENTED_EDGE('',*,*,#7164,.F.);
#10258=ORIENTED_EDGE('',*,*,#7165,.T.);
#10259=ORIENTED_EDGE('',*,*,#7161,.T.);
#10260=ORIENTED_EDGE('',*,*,#7166,.T.);
#10261=ORIENTED_EDGE('',*,*,#7167,.F.);
#10262=ORIENTED_EDGE('',*,*,#7168,.T.);
#10263=ORIENTED_EDGE('',*,*,#7169,.F.);
#10264=ORIENTED_EDGE('',*,*,#7170,.F.);
#10265=ORIENTED_EDGE('',*,*,#7171,.T.);
#10266=ORIENTED_EDGE('',*,*,#7167,.T.);
#10267=ORIENTED_EDGE('',*,*,#7172,.F.);
#10268=ORIENTED_EDGE('',*,*,#7173,.F.);
#10269=ORIENTED_EDGE('',*,*,#7174,.F.);
#10270=ORIENTED_EDGE('',*,*,#7175,.T.);
#10271=ORIENTED_EDGE('',*,*,#7170,.T.);
#10272=ORIENTED_EDGE('',*,*,#7176,.F.);
#10273=ORIENTED_EDGE('',*,*,#7177,.F.);
#10274=ORIENTED_EDGE('',*,*,#7178,.T.);
#10275=ORIENTED_EDGE('',*,*,#7174,.T.);
#10276=ORIENTED_EDGE('',*,*,#7179,.F.);
#10277=ORIENTED_EDGE('',*,*,#7180,.F.);
#10278=ORIENTED_EDGE('',*,*,#7181,.T.);
#10279=ORIENTED_EDGE('',*,*,#7177,.T.);
#10280=ORIENTED_EDGE('',*,*,#7182,.F.);
#10281=ORIENTED_EDGE('',*,*,#7183,.F.);
#10282=ORIENTED_EDGE('',*,*,#7184,.T.);
#10283=ORIENTED_EDGE('',*,*,#7180,.T.);
#10284=ORIENTED_EDGE('',*,*,#7185,.F.);
#10285=ORIENTED_EDGE('',*,*,#7186,.F.);
#10286=ORIENTED_EDGE('',*,*,#7187,.T.);
#10287=ORIENTED_EDGE('',*,*,#7183,.T.);
#10288=ORIENTED_EDGE('',*,*,#7188,.F.);
#10289=ORIENTED_EDGE('',*,*,#7189,.F.);
#10290=ORIENTED_EDGE('',*,*,#7190,.T.);
#10291=ORIENTED_EDGE('',*,*,#7186,.T.);
#10292=ORIENTED_EDGE('',*,*,#7191,.F.);
#10293=ORIENTED_EDGE('',*,*,#7192,.F.);
#10294=ORIENTED_EDGE('',*,*,#7193,.T.);
#10295=ORIENTED_EDGE('',*,*,#7189,.T.);
#10296=ORIENTED_EDGE('',*,*,#7194,.F.);
#10297=ORIENTED_EDGE('',*,*,#7195,.F.);
#10298=ORIENTED_EDGE('',*,*,#7196,.T.);
#10299=ORIENTED_EDGE('',*,*,#7192,.T.);
#10300=ORIENTED_EDGE('',*,*,#7197,.F.);
#10301=ORIENTED_EDGE('',*,*,#7198,.F.);
#10302=ORIENTED_EDGE('',*,*,#7199,.T.);
#10303=ORIENTED_EDGE('',*,*,#7195,.T.);
#10304=ORIENTED_EDGE('',*,*,#7200,.F.);
#10305=ORIENTED_EDGE('',*,*,#7201,.F.);
#10306=ORIENTED_EDGE('',*,*,#7202,.T.);
#10307=ORIENTED_EDGE('',*,*,#7198,.T.);
#10308=ORIENTED_EDGE('',*,*,#7203,.F.);
#10309=ORIENTED_EDGE('',*,*,#7204,.F.);
#10310=ORIENTED_EDGE('',*,*,#7205,.T.);
#10311=ORIENTED_EDGE('',*,*,#7201,.T.);
#10312=ORIENTED_EDGE('',*,*,#7206,.F.);
#10313=ORIENTED_EDGE('',*,*,#7207,.F.);
#10314=ORIENTED_EDGE('',*,*,#7208,.T.);
#10315=ORIENTED_EDGE('',*,*,#7204,.T.);
#10316=ORIENTED_EDGE('',*,*,#7209,.F.);
#10317=ORIENTED_EDGE('',*,*,#7210,.F.);
#10318=ORIENTED_EDGE('',*,*,#7211,.T.);
#10319=ORIENTED_EDGE('',*,*,#7207,.T.);
#10320=ORIENTED_EDGE('',*,*,#7212,.F.);
#10321=ORIENTED_EDGE('',*,*,#7213,.F.);
#10322=ORIENTED_EDGE('',*,*,#7214,.T.);
#10323=ORIENTED_EDGE('',*,*,#7210,.T.);
#10324=ORIENTED_EDGE('',*,*,#7215,.F.);
#10325=ORIENTED_EDGE('',*,*,#7216,.F.);
#10326=ORIENTED_EDGE('',*,*,#7217,.T.);
#10327=ORIENTED_EDGE('',*,*,#7213,.T.);
#10328=ORIENTED_EDGE('',*,*,#7218,.F.);
#10329=ORIENTED_EDGE('',*,*,#7219,.F.);
#10330=ORIENTED_EDGE('',*,*,#7220,.T.);
#10331=ORIENTED_EDGE('',*,*,#7216,.T.);
#10332=ORIENTED_EDGE('',*,*,#7221,.F.);
#10333=ORIENTED_EDGE('',*,*,#7222,.F.);
#10334=ORIENTED_EDGE('',*,*,#7223,.T.);
#10335=ORIENTED_EDGE('',*,*,#7219,.T.);
#10336=ORIENTED_EDGE('',*,*,#7224,.F.);
#10337=ORIENTED_EDGE('',*,*,#7225,.F.);
#10338=ORIENTED_EDGE('',*,*,#7226,.T.);
#10339=ORIENTED_EDGE('',*,*,#7222,.T.);
#10340=ORIENTED_EDGE('',*,*,#7227,.F.);
#10341=ORIENTED_EDGE('',*,*,#7228,.F.);
#10342=ORIENTED_EDGE('',*,*,#7229,.T.);
#10343=ORIENTED_EDGE('',*,*,#7225,.T.);
#10344=ORIENTED_EDGE('',*,*,#7230,.F.);
#10345=ORIENTED_EDGE('',*,*,#7231,.F.);
#10346=ORIENTED_EDGE('',*,*,#7232,.T.);
#10347=ORIENTED_EDGE('',*,*,#7228,.T.);
#10348=ORIENTED_EDGE('',*,*,#7233,.F.);
#10349=ORIENTED_EDGE('',*,*,#7234,.F.);
#10350=ORIENTED_EDGE('',*,*,#7235,.T.);
#10351=ORIENTED_EDGE('',*,*,#7231,.T.);
#10352=ORIENTED_EDGE('',*,*,#7236,.F.);
#10353=ORIENTED_EDGE('',*,*,#7237,.F.);
#10354=ORIENTED_EDGE('',*,*,#7238,.T.);
#10355=ORIENTED_EDGE('',*,*,#7234,.T.);
#10356=ORIENTED_EDGE('',*,*,#7239,.F.);
#10357=ORIENTED_EDGE('',*,*,#7240,.F.);
#10358=ORIENTED_EDGE('',*,*,#7241,.F.);
#10359=ORIENTED_EDGE('',*,*,#7166,.F.);
#10360=ORIENTED_EDGE('',*,*,#7163,.F.);
#10361=ORIENTED_EDGE('',*,*,#7160,.F.);
#10362=ORIENTED_EDGE('',*,*,#7157,.F.);
#10363=ORIENTED_EDGE('',*,*,#7154,.F.);
#10364=ORIENTED_EDGE('',*,*,#7151,.F.);
#10365=ORIENTED_EDGE('',*,*,#7148,.F.);
#10366=ORIENTED_EDGE('',*,*,#7145,.F.);
#10367=ORIENTED_EDGE('',*,*,#7142,.F.);
#10368=ORIENTED_EDGE('',*,*,#7139,.F.);
#10369=ORIENTED_EDGE('',*,*,#7136,.F.);
#10370=ORIENTED_EDGE('',*,*,#7133,.F.);
#10371=ORIENTED_EDGE('',*,*,#7130,.F.);
#10372=ORIENTED_EDGE('',*,*,#7127,.F.);
#10373=ORIENTED_EDGE('',*,*,#7124,.F.);
#10374=ORIENTED_EDGE('',*,*,#7121,.F.);
#10375=ORIENTED_EDGE('',*,*,#7118,.F.);
#10376=ORIENTED_EDGE('',*,*,#7115,.F.);
#10377=ORIENTED_EDGE('',*,*,#7112,.F.);
#10378=ORIENTED_EDGE('',*,*,#7109,.F.);
#10379=ORIENTED_EDGE('',*,*,#7106,.F.);
#10380=ORIENTED_EDGE('',*,*,#7103,.F.);
#10381=ORIENTED_EDGE('',*,*,#7100,.F.);
#10382=ORIENTED_EDGE('',*,*,#7097,.F.);
#10383=ORIENTED_EDGE('',*,*,#7242,.F.);
#10384=ORIENTED_EDGE('',*,*,#7243,.T.);
#10385=ORIENTED_EDGE('',*,*,#7239,.T.);
#10386=ORIENTED_EDGE('',*,*,#7236,.T.);
#10387=ORIENTED_EDGE('',*,*,#7233,.T.);
#10388=ORIENTED_EDGE('',*,*,#7230,.T.);
#10389=ORIENTED_EDGE('',*,*,#7227,.T.);
#10390=ORIENTED_EDGE('',*,*,#7224,.T.);
#10391=ORIENTED_EDGE('',*,*,#7221,.T.);
#10392=ORIENTED_EDGE('',*,*,#7218,.T.);
#10393=ORIENTED_EDGE('',*,*,#7215,.T.);
#10394=ORIENTED_EDGE('',*,*,#7212,.T.);
#10395=ORIENTED_EDGE('',*,*,#7209,.T.);
#10396=ORIENTED_EDGE('',*,*,#7206,.T.);
#10397=ORIENTED_EDGE('',*,*,#7203,.T.);
#10398=ORIENTED_EDGE('',*,*,#7200,.T.);
#10399=ORIENTED_EDGE('',*,*,#7197,.T.);
#10400=ORIENTED_EDGE('',*,*,#7194,.T.);
#10401=ORIENTED_EDGE('',*,*,#7191,.T.);
#10402=ORIENTED_EDGE('',*,*,#7188,.T.);
#10403=ORIENTED_EDGE('',*,*,#7185,.T.);
#10404=ORIENTED_EDGE('',*,*,#7182,.T.);
#10405=ORIENTED_EDGE('',*,*,#7179,.T.);
#10406=ORIENTED_EDGE('',*,*,#7176,.T.);
#10407=ORIENTED_EDGE('',*,*,#7173,.T.);
#10408=ORIENTED_EDGE('',*,*,#7244,.T.);
#10409=ORIENTED_EDGE('',*,*,#7245,.T.);
#10410=ORIENTED_EDGE('',*,*,#7246,.T.);
#10411=ORIENTED_EDGE('',*,*,#7247,.T.);
#10412=ORIENTED_EDGE('',*,*,#7242,.T.);
#10413=ORIENTED_EDGE('',*,*,#7237,.T.);
#10414=ORIENTED_EDGE('',*,*,#7243,.F.);
#10415=ORIENTED_EDGE('',*,*,#7247,.F.);
#10416=ORIENTED_EDGE('',*,*,#7248,.T.);
#10417=ORIENTED_EDGE('',*,*,#7249,.F.);
#10418=ORIENTED_EDGE('',*,*,#7168,.F.);
#10419=ORIENTED_EDGE('',*,*,#7171,.F.);
#10420=ORIENTED_EDGE('',*,*,#7175,.F.);
#10421=ORIENTED_EDGE('',*,*,#7178,.F.);
#10422=ORIENTED_EDGE('',*,*,#7181,.F.);
#10423=ORIENTED_EDGE('',*,*,#7184,.F.);
#10424=ORIENTED_EDGE('',*,*,#7187,.F.);
#10425=ORIENTED_EDGE('',*,*,#7190,.F.);
#10426=ORIENTED_EDGE('',*,*,#7193,.F.);
#10427=ORIENTED_EDGE('',*,*,#7196,.F.);
#10428=ORIENTED_EDGE('',*,*,#7199,.F.);
#10429=ORIENTED_EDGE('',*,*,#7202,.F.);
#10430=ORIENTED_EDGE('',*,*,#7205,.F.);
#10431=ORIENTED_EDGE('',*,*,#7208,.F.);
#10432=ORIENTED_EDGE('',*,*,#7211,.F.);
#10433=ORIENTED_EDGE('',*,*,#7214,.F.);
#10434=ORIENTED_EDGE('',*,*,#7217,.F.);
#10435=ORIENTED_EDGE('',*,*,#7220,.F.);
#10436=ORIENTED_EDGE('',*,*,#7223,.F.);
#10437=ORIENTED_EDGE('',*,*,#7226,.F.);
#10438=ORIENTED_EDGE('',*,*,#7229,.F.);
#10439=ORIENTED_EDGE('',*,*,#7232,.F.);
#10440=ORIENTED_EDGE('',*,*,#7235,.F.);
#10441=ORIENTED_EDGE('',*,*,#7238,.F.);
#10442=ORIENTED_EDGE('',*,*,#7248,.F.);
#10443=ORIENTED_EDGE('',*,*,#7246,.F.);
#10444=ORIENTED_EDGE('',*,*,#7095,.F.);
#10445=ORIENTED_EDGE('',*,*,#7099,.F.);
#10446=ORIENTED_EDGE('',*,*,#7102,.F.);
#10447=ORIENTED_EDGE('',*,*,#7105,.F.);
#10448=ORIENTED_EDGE('',*,*,#7108,.F.);
#10449=ORIENTED_EDGE('',*,*,#7111,.F.);
#10450=ORIENTED_EDGE('',*,*,#7114,.F.);
#10451=ORIENTED_EDGE('',*,*,#7117,.F.);
#10452=ORIENTED_EDGE('',*,*,#7120,.F.);
#10453=ORIENTED_EDGE('',*,*,#7123,.F.);
#10454=ORIENTED_EDGE('',*,*,#7126,.F.);
#10455=ORIENTED_EDGE('',*,*,#7129,.F.);
#10456=ORIENTED_EDGE('',*,*,#7132,.F.);
#10457=ORIENTED_EDGE('',*,*,#7135,.F.);
#10458=ORIENTED_EDGE('',*,*,#7138,.F.);
#10459=ORIENTED_EDGE('',*,*,#7141,.F.);
#10460=ORIENTED_EDGE('',*,*,#7144,.F.);
#10461=ORIENTED_EDGE('',*,*,#7147,.F.);
#10462=ORIENTED_EDGE('',*,*,#7150,.F.);
#10463=ORIENTED_EDGE('',*,*,#7153,.F.);
#10464=ORIENTED_EDGE('',*,*,#7156,.F.);
#10465=ORIENTED_EDGE('',*,*,#7159,.F.);
#10466=ORIENTED_EDGE('',*,*,#7162,.F.);
#10467=ORIENTED_EDGE('',*,*,#7165,.F.);
#10468=ORIENTED_EDGE('',*,*,#7250,.F.);
#10469=ORIENTED_EDGE('',*,*,#7251,.T.);
#10470=ORIENTED_EDGE('',*,*,#7252,.F.);
#10471=ORIENTED_EDGE('',*,*,#7251,.F.);
#10472=ORIENTED_EDGE('',*,*,#7253,.F.);
#10473=ORIENTED_EDGE('',*,*,#7254,.T.);
#10474=ORIENTED_EDGE('',*,*,#7255,.T.);
#10475=ORIENTED_EDGE('',*,*,#7256,.F.);
#10476=ORIENTED_EDGE('',*,*,#7257,.F.);
#10477=ORIENTED_EDGE('',*,*,#7258,.T.);
#10478=ORIENTED_EDGE('',*,*,#7259,.T.);
#10479=ORIENTED_EDGE('',*,*,#7254,.F.);
#10480=ORIENTED_EDGE('',*,*,#7260,.F.);
#10481=ORIENTED_EDGE('',*,*,#7261,.T.);
#10482=ORIENTED_EDGE('',*,*,#7262,.T.);
#10483=ORIENTED_EDGE('',*,*,#7258,.F.);
#10484=ORIENTED_EDGE('',*,*,#7263,.F.);
#10485=ORIENTED_EDGE('',*,*,#7264,.T.);
#10486=ORIENTED_EDGE('',*,*,#7265,.T.);
#10487=ORIENTED_EDGE('',*,*,#7261,.F.);
#10488=ORIENTED_EDGE('',*,*,#7266,.F.);
#10489=ORIENTED_EDGE('',*,*,#7267,.T.);
#10490=ORIENTED_EDGE('',*,*,#7268,.T.);
#10491=ORIENTED_EDGE('',*,*,#7264,.F.);
#10492=ORIENTED_EDGE('',*,*,#7269,.F.);
#10493=ORIENTED_EDGE('',*,*,#7256,.T.);
#10494=ORIENTED_EDGE('',*,*,#7270,.T.);
#10495=ORIENTED_EDGE('',*,*,#7267,.F.);
#10496=ORIENTED_EDGE('',*,*,#7270,.F.);
#10497=ORIENTED_EDGE('',*,*,#7255,.F.);
#10498=ORIENTED_EDGE('',*,*,#7259,.F.);
#10499=ORIENTED_EDGE('',*,*,#7262,.F.);
#10500=ORIENTED_EDGE('',*,*,#7265,.F.);
#10501=ORIENTED_EDGE('',*,*,#7268,.F.);
#10502=ORIENTED_EDGE('',*,*,#7252,.T.);
#10503=ORIENTED_EDGE('',*,*,#7271,.F.);
#10504=ORIENTED_EDGE('',*,*,#7272,.T.);
#10505=ORIENTED_EDGE('',*,*,#7273,.F.);
#10506=ORIENTED_EDGE('',*,*,#7274,.F.);
#10507=ORIENTED_EDGE('',*,*,#7275,.F.);
#10508=ORIENTED_EDGE('',*,*,#7274,.T.);
#10509=ORIENTED_EDGE('',*,*,#7276,.T.);
#10510=ORIENTED_EDGE('',*,*,#7277,.F.);
#10511=ORIENTED_EDGE('',*,*,#7276,.F.);
#10512=ORIENTED_EDGE('',*,*,#7273,.T.);
#10513=ORIENTED_EDGE('',*,*,#7278,.T.);
#10514=ORIENTED_EDGE('',*,*,#7279,.F.);
#10515=ORIENTED_EDGE('',*,*,#7278,.F.);
#10516=ORIENTED_EDGE('',*,*,#7272,.F.);
#10517=ORIENTED_EDGE('',*,*,#7280,.F.);
#10518=ORIENTED_EDGE('',*,*,#7281,.T.);
#10519=ORIENTED_EDGE('',*,*,#7282,.F.);
#10520=ORIENTED_EDGE('',*,*,#7283,.F.);
#10521=ORIENTED_EDGE('',*,*,#7284,.F.);
#10522=ORIENTED_EDGE('',*,*,#7283,.T.);
#10523=ORIENTED_EDGE('',*,*,#7285,.T.);
#10524=ORIENTED_EDGE('',*,*,#7286,.F.);
#10525=ORIENTED_EDGE('',*,*,#7285,.F.);
#10526=ORIENTED_EDGE('',*,*,#7282,.T.);
#10527=ORIENTED_EDGE('',*,*,#7287,.T.);
#10528=ORIENTED_EDGE('',*,*,#7288,.F.);
#10529=ORIENTED_EDGE('',*,*,#7287,.F.);
#10530=ORIENTED_EDGE('',*,*,#7281,.F.);
#10531=ORIENTED_EDGE('',*,*,#7289,.F.);
#10532=ORIENTED_EDGE('',*,*,#7290,.T.);
#10533=ORIENTED_EDGE('',*,*,#7291,.F.);
#10534=ORIENTED_EDGE('',*,*,#7292,.F.);
#10535=ORIENTED_EDGE('',*,*,#7293,.F.);
#10536=ORIENTED_EDGE('',*,*,#7292,.T.);
#10537=ORIENTED_EDGE('',*,*,#7294,.T.);
#10538=ORIENTED_EDGE('',*,*,#7295,.F.);
#10539=ORIENTED_EDGE('',*,*,#7294,.F.);
#10540=ORIENTED_EDGE('',*,*,#7291,.T.);
#10541=ORIENTED_EDGE('',*,*,#7296,.T.);
#10542=ORIENTED_EDGE('',*,*,#7297,.F.);
#10543=ORIENTED_EDGE('',*,*,#7296,.F.);
#10544=ORIENTED_EDGE('',*,*,#7290,.F.);
#10545=ORIENTED_EDGE('',*,*,#7298,.F.);
#10546=ORIENTED_EDGE('',*,*,#7299,.T.);
#10547=ORIENTED_EDGE('',*,*,#7300,.F.);
#10548=ORIENTED_EDGE('',*,*,#7301,.F.);
#10549=ORIENTED_EDGE('',*,*,#7302,.F.);
#10550=ORIENTED_EDGE('',*,*,#7301,.T.);
#10551=ORIENTED_EDGE('',*,*,#7303,.T.);
#10552=ORIENTED_EDGE('',*,*,#7304,.F.);
#10553=ORIENTED_EDGE('',*,*,#7303,.F.);
#10554=ORIENTED_EDGE('',*,*,#7300,.T.);
#10555=ORIENTED_EDGE('',*,*,#7305,.T.);
#10556=ORIENTED_EDGE('',*,*,#7306,.F.);
#10557=ORIENTED_EDGE('',*,*,#7305,.F.);
#10558=ORIENTED_EDGE('',*,*,#7299,.F.);
#10559=ORIENTED_EDGE('',*,*,#7307,.F.);
#10560=ORIENTED_EDGE('',*,*,#7308,.T.);
#10561=ORIENTED_EDGE('',*,*,#7309,.F.);
#10562=ORIENTED_EDGE('',*,*,#7310,.F.);
#10563=ORIENTED_EDGE('',*,*,#7311,.F.);
#10564=ORIENTED_EDGE('',*,*,#7310,.T.);
#10565=ORIENTED_EDGE('',*,*,#7312,.T.);
#10566=ORIENTED_EDGE('',*,*,#7313,.F.);
#10567=ORIENTED_EDGE('',*,*,#7312,.F.);
#10568=ORIENTED_EDGE('',*,*,#7309,.T.);
#10569=ORIENTED_EDGE('',*,*,#7314,.T.);
#10570=ORIENTED_EDGE('',*,*,#7315,.F.);
#10571=ORIENTED_EDGE('',*,*,#7314,.F.);
#10572=ORIENTED_EDGE('',*,*,#7308,.F.);
#10573=ORIENTED_EDGE('',*,*,#7316,.F.);
#10574=ORIENTED_EDGE('',*,*,#7317,.T.);
#10575=ORIENTED_EDGE('',*,*,#7318,.F.);
#10576=ORIENTED_EDGE('',*,*,#7319,.F.);
#10577=ORIENTED_EDGE('',*,*,#7320,.F.);
#10578=ORIENTED_EDGE('',*,*,#7319,.T.);
#10579=ORIENTED_EDGE('',*,*,#7321,.T.);
#10580=ORIENTED_EDGE('',*,*,#7322,.F.);
#10581=ORIENTED_EDGE('',*,*,#7321,.F.);
#10582=ORIENTED_EDGE('',*,*,#7318,.T.);
#10583=ORIENTED_EDGE('',*,*,#7323,.T.);
#10584=ORIENTED_EDGE('',*,*,#7324,.F.);
#10585=ORIENTED_EDGE('',*,*,#7323,.F.);
#10586=ORIENTED_EDGE('',*,*,#7317,.F.);
#10587=ORIENTED_EDGE('',*,*,#7325,.F.);
#10588=ORIENTED_EDGE('',*,*,#7326,.T.);
#10589=ORIENTED_EDGE('',*,*,#7327,.F.);
#10590=ORIENTED_EDGE('',*,*,#7328,.F.);
#10591=ORIENTED_EDGE('',*,*,#7329,.F.);
#10592=ORIENTED_EDGE('',*,*,#7328,.T.);
#10593=ORIENTED_EDGE('',*,*,#7330,.T.);
#10594=ORIENTED_EDGE('',*,*,#7331,.F.);
#10595=ORIENTED_EDGE('',*,*,#7330,.F.);
#10596=ORIENTED_EDGE('',*,*,#7327,.T.);
#10597=ORIENTED_EDGE('',*,*,#7332,.T.);
#10598=ORIENTED_EDGE('',*,*,#7333,.F.);
#10599=ORIENTED_EDGE('',*,*,#7332,.F.);
#10600=ORIENTED_EDGE('',*,*,#7326,.F.);
#10601=ORIENTED_EDGE('',*,*,#7334,.F.);
#10602=ORIENTED_EDGE('',*,*,#7335,.T.);
#10603=ORIENTED_EDGE('',*,*,#7336,.F.);
#10604=ORIENTED_EDGE('',*,*,#7337,.F.);
#10605=ORIENTED_EDGE('',*,*,#7338,.F.);
#10606=ORIENTED_EDGE('',*,*,#7337,.T.);
#10607=ORIENTED_EDGE('',*,*,#7339,.T.);
#10608=ORIENTED_EDGE('',*,*,#7340,.F.);
#10609=ORIENTED_EDGE('',*,*,#7339,.F.);
#10610=ORIENTED_EDGE('',*,*,#7336,.T.);
#10611=ORIENTED_EDGE('',*,*,#7341,.T.);
#10612=ORIENTED_EDGE('',*,*,#7342,.F.);
#10613=ORIENTED_EDGE('',*,*,#7341,.F.);
#10614=ORIENTED_EDGE('',*,*,#7335,.F.);
#10615=ORIENTED_EDGE('',*,*,#7343,.F.);
#10616=ORIENTED_EDGE('',*,*,#7344,.T.);
#10617=ORIENTED_EDGE('',*,*,#7345,.F.);
#10618=ORIENTED_EDGE('',*,*,#7346,.F.);
#10619=ORIENTED_EDGE('',*,*,#7347,.F.);
#10620=ORIENTED_EDGE('',*,*,#7346,.T.);
#10621=ORIENTED_EDGE('',*,*,#7348,.T.);
#10622=ORIENTED_EDGE('',*,*,#7349,.F.);
#10623=ORIENTED_EDGE('',*,*,#7350,.F.);
#10624=ORIENTED_EDGE('',*,*,#7348,.F.);
#10625=ORIENTED_EDGE('',*,*,#7345,.T.);
#10626=ORIENTED_EDGE('',*,*,#7351,.T.);
#10627=ORIENTED_EDGE('',*,*,#7352,.F.);
#10628=ORIENTED_EDGE('',*,*,#7351,.F.);
#10629=ORIENTED_EDGE('',*,*,#7344,.F.);
#10630=ORIENTED_EDGE('',*,*,#7353,.F.);
#10631=ORIENTED_EDGE('',*,*,#7354,.F.);
#10632=ORIENTED_EDGE('',*,*,#7355,.T.);
#10633=ORIENTED_EDGE('',*,*,#7356,.F.);
#10634=ORIENTED_EDGE('',*,*,#7357,.F.);
#10635=ORIENTED_EDGE('',*,*,#7358,.F.);
#10636=ORIENTED_EDGE('',*,*,#7357,.T.);
#10637=ORIENTED_EDGE('',*,*,#7359,.T.);
#10638=ORIENTED_EDGE('',*,*,#7360,.F.);
#10639=ORIENTED_EDGE('',*,*,#7359,.F.);
#10640=ORIENTED_EDGE('',*,*,#7356,.T.);
#10641=ORIENTED_EDGE('',*,*,#7361,.T.);
#10642=ORIENTED_EDGE('',*,*,#7362,.F.);
#10643=ORIENTED_EDGE('',*,*,#7361,.F.);
#10644=ORIENTED_EDGE('',*,*,#7355,.F.);
#10645=ORIENTED_EDGE('',*,*,#7363,.F.);
#10646=ORIENTED_EDGE('',*,*,#7364,.T.);
#10647=ORIENTED_EDGE('',*,*,#7365,.F.);
#10648=ORIENTED_EDGE('',*,*,#7366,.F.);
#10649=ORIENTED_EDGE('',*,*,#7367,.F.);
#10650=ORIENTED_EDGE('',*,*,#7366,.T.);
#10651=ORIENTED_EDGE('',*,*,#7368,.T.);
#10652=ORIENTED_EDGE('',*,*,#7369,.F.);
#10653=ORIENTED_EDGE('',*,*,#7368,.F.);
#10654=ORIENTED_EDGE('',*,*,#7365,.T.);
#10655=ORIENTED_EDGE('',*,*,#7370,.T.);
#10656=ORIENTED_EDGE('',*,*,#7371,.F.);
#10657=ORIENTED_EDGE('',*,*,#7370,.F.);
#10658=ORIENTED_EDGE('',*,*,#7364,.F.);
#10659=ORIENTED_EDGE('',*,*,#7372,.F.);
#10660=ORIENTED_EDGE('',*,*,#7373,.T.);
#10661=ORIENTED_EDGE('',*,*,#7374,.F.);
#10662=ORIENTED_EDGE('',*,*,#7375,.F.);
#10663=ORIENTED_EDGE('',*,*,#7376,.F.);
#10664=ORIENTED_EDGE('',*,*,#7375,.T.);
#10665=ORIENTED_EDGE('',*,*,#7377,.T.);
#10666=ORIENTED_EDGE('',*,*,#7378,.F.);
#10667=ORIENTED_EDGE('',*,*,#7377,.F.);
#10668=ORIENTED_EDGE('',*,*,#7374,.T.);
#10669=ORIENTED_EDGE('',*,*,#7379,.T.);
#10670=ORIENTED_EDGE('',*,*,#7380,.F.);
#10671=ORIENTED_EDGE('',*,*,#7379,.F.);
#10672=ORIENTED_EDGE('',*,*,#7373,.F.);
#10673=ORIENTED_EDGE('',*,*,#7381,.F.);
#10674=ORIENTED_EDGE('',*,*,#7382,.T.);
#10675=ORIENTED_EDGE('',*,*,#7383,.F.);
#10676=ORIENTED_EDGE('',*,*,#7384,.F.);
#10677=ORIENTED_EDGE('',*,*,#7385,.F.);
#10678=ORIENTED_EDGE('',*,*,#7384,.T.);
#10679=ORIENTED_EDGE('',*,*,#7386,.T.);
#10680=ORIENTED_EDGE('',*,*,#7387,.F.);
#10681=ORIENTED_EDGE('',*,*,#7386,.F.);
#10682=ORIENTED_EDGE('',*,*,#7383,.T.);
#10683=ORIENTED_EDGE('',*,*,#7388,.T.);
#10684=ORIENTED_EDGE('',*,*,#7389,.F.);
#10685=ORIENTED_EDGE('',*,*,#7388,.F.);
#10686=ORIENTED_EDGE('',*,*,#7382,.F.);
#10687=ORIENTED_EDGE('',*,*,#7390,.F.);
#10688=ORIENTED_EDGE('',*,*,#7391,.T.);
#10689=ORIENTED_EDGE('',*,*,#7392,.F.);
#10690=ORIENTED_EDGE('',*,*,#7393,.F.);
#10691=ORIENTED_EDGE('',*,*,#7394,.F.);
#10692=ORIENTED_EDGE('',*,*,#7393,.T.);
#10693=ORIENTED_EDGE('',*,*,#7395,.T.);
#10694=ORIENTED_EDGE('',*,*,#7396,.F.);
#10695=ORIENTED_EDGE('',*,*,#7395,.F.);
#10696=ORIENTED_EDGE('',*,*,#7392,.T.);
#10697=ORIENTED_EDGE('',*,*,#7397,.T.);
#10698=ORIENTED_EDGE('',*,*,#7398,.F.);
#10699=ORIENTED_EDGE('',*,*,#7397,.F.);
#10700=ORIENTED_EDGE('',*,*,#7391,.F.);
#10701=ORIENTED_EDGE('',*,*,#7399,.F.);
#10702=ORIENTED_EDGE('',*,*,#7400,.T.);
#10703=ORIENTED_EDGE('',*,*,#7401,.F.);
#10704=ORIENTED_EDGE('',*,*,#7402,.F.);
#10705=ORIENTED_EDGE('',*,*,#7403,.F.);
#10706=ORIENTED_EDGE('',*,*,#7402,.T.);
#10707=ORIENTED_EDGE('',*,*,#7404,.T.);
#10708=ORIENTED_EDGE('',*,*,#7405,.F.);
#10709=ORIENTED_EDGE('',*,*,#7404,.F.);
#10710=ORIENTED_EDGE('',*,*,#7401,.T.);
#10711=ORIENTED_EDGE('',*,*,#7406,.T.);
#10712=ORIENTED_EDGE('',*,*,#7407,.F.);
#10713=ORIENTED_EDGE('',*,*,#7406,.F.);
#10714=ORIENTED_EDGE('',*,*,#7400,.F.);
#10715=ORIENTED_EDGE('',*,*,#7408,.F.);
#10716=ORIENTED_EDGE('',*,*,#7409,.T.);
#10717=ORIENTED_EDGE('',*,*,#7410,.F.);
#10718=ORIENTED_EDGE('',*,*,#7411,.F.);
#10719=ORIENTED_EDGE('',*,*,#7412,.F.);
#10720=ORIENTED_EDGE('',*,*,#7411,.T.);
#10721=ORIENTED_EDGE('',*,*,#7413,.T.);
#10722=ORIENTED_EDGE('',*,*,#7414,.F.);
#10723=ORIENTED_EDGE('',*,*,#7413,.F.);
#10724=ORIENTED_EDGE('',*,*,#7410,.T.);
#10725=ORIENTED_EDGE('',*,*,#7415,.T.);
#10726=ORIENTED_EDGE('',*,*,#7416,.F.);
#10727=ORIENTED_EDGE('',*,*,#7415,.F.);
#10728=ORIENTED_EDGE('',*,*,#7409,.F.);
#10729=ORIENTED_EDGE('',*,*,#7417,.F.);
#10730=ORIENTED_EDGE('',*,*,#7418,.T.);
#10731=ORIENTED_EDGE('',*,*,#7419,.F.);
#10732=ORIENTED_EDGE('',*,*,#7420,.F.);
#10733=ORIENTED_EDGE('',*,*,#7421,.F.);
#10734=ORIENTED_EDGE('',*,*,#7420,.T.);
#10735=ORIENTED_EDGE('',*,*,#7422,.T.);
#10736=ORIENTED_EDGE('',*,*,#7423,.F.);
#10737=ORIENTED_EDGE('',*,*,#7422,.F.);
#10738=ORIENTED_EDGE('',*,*,#7419,.T.);
#10739=ORIENTED_EDGE('',*,*,#7424,.T.);
#10740=ORIENTED_EDGE('',*,*,#7425,.F.);
#10741=ORIENTED_EDGE('',*,*,#7424,.F.);
#10742=ORIENTED_EDGE('',*,*,#7418,.F.);
#10743=ORIENTED_EDGE('',*,*,#7426,.F.);
#10744=ORIENTED_EDGE('',*,*,#7427,.T.);
#10745=ORIENTED_EDGE('',*,*,#7428,.F.);
#10746=ORIENTED_EDGE('',*,*,#7429,.F.);
#10747=ORIENTED_EDGE('',*,*,#7430,.F.);
#10748=ORIENTED_EDGE('',*,*,#7429,.T.);
#10749=ORIENTED_EDGE('',*,*,#7431,.T.);
#10750=ORIENTED_EDGE('',*,*,#7432,.F.);
#10751=ORIENTED_EDGE('',*,*,#7431,.F.);
#10752=ORIENTED_EDGE('',*,*,#7428,.T.);
#10753=ORIENTED_EDGE('',*,*,#7433,.T.);
#10754=ORIENTED_EDGE('',*,*,#7434,.F.);
#10755=ORIENTED_EDGE('',*,*,#7433,.F.);
#10756=ORIENTED_EDGE('',*,*,#7427,.F.);
#10757=ORIENTED_EDGE('',*,*,#7435,.F.);
#10758=ORIENTED_EDGE('',*,*,#7436,.T.);
#10759=ORIENTED_EDGE('',*,*,#7437,.F.);
#10760=ORIENTED_EDGE('',*,*,#7438,.F.);
#10761=ORIENTED_EDGE('',*,*,#7439,.F.);
#10762=ORIENTED_EDGE('',*,*,#7438,.T.);
#10763=ORIENTED_EDGE('',*,*,#7440,.T.);
#10764=ORIENTED_EDGE('',*,*,#7441,.F.);
#10765=ORIENTED_EDGE('',*,*,#7440,.F.);
#10766=ORIENTED_EDGE('',*,*,#7437,.T.);
#10767=ORIENTED_EDGE('',*,*,#7442,.T.);
#10768=ORIENTED_EDGE('',*,*,#7443,.F.);
#10769=ORIENTED_EDGE('',*,*,#7442,.F.);
#10770=ORIENTED_EDGE('',*,*,#7436,.F.);
#10771=ORIENTED_EDGE('',*,*,#7444,.F.);
#10772=ORIENTED_EDGE('',*,*,#7445,.T.);
#10773=ORIENTED_EDGE('',*,*,#7446,.F.);
#10774=ORIENTED_EDGE('',*,*,#7447,.F.);
#10775=ORIENTED_EDGE('',*,*,#7448,.F.);
#10776=ORIENTED_EDGE('',*,*,#7447,.T.);
#10777=ORIENTED_EDGE('',*,*,#7449,.T.);
#10778=ORIENTED_EDGE('',*,*,#7450,.F.);
#10779=ORIENTED_EDGE('',*,*,#7449,.F.);
#10780=ORIENTED_EDGE('',*,*,#7446,.T.);
#10781=ORIENTED_EDGE('',*,*,#7451,.T.);
#10782=ORIENTED_EDGE('',*,*,#7452,.F.);
#10783=ORIENTED_EDGE('',*,*,#7451,.F.);
#10784=ORIENTED_EDGE('',*,*,#7445,.F.);
#10785=ORIENTED_EDGE('',*,*,#7453,.F.);
#10786=ORIENTED_EDGE('',*,*,#7454,.T.);
#10787=ORIENTED_EDGE('',*,*,#7455,.F.);
#10788=ORIENTED_EDGE('',*,*,#7456,.F.);
#10789=ORIENTED_EDGE('',*,*,#7457,.F.);
#10790=ORIENTED_EDGE('',*,*,#7456,.T.);
#10791=ORIENTED_EDGE('',*,*,#7458,.T.);
#10792=ORIENTED_EDGE('',*,*,#7459,.F.);
#10793=ORIENTED_EDGE('',*,*,#7458,.F.);
#10794=ORIENTED_EDGE('',*,*,#7455,.T.);
#10795=ORIENTED_EDGE('',*,*,#7460,.T.);
#10796=ORIENTED_EDGE('',*,*,#7461,.F.);
#10797=ORIENTED_EDGE('',*,*,#7460,.F.);
#10798=ORIENTED_EDGE('',*,*,#7454,.F.);
#10799=ORIENTED_EDGE('',*,*,#7462,.F.);
#10800=ORIENTED_EDGE('',*,*,#7463,.T.);
#10801=ORIENTED_EDGE('',*,*,#7464,.F.);
#10802=ORIENTED_EDGE('',*,*,#7465,.F.);
#10803=ORIENTED_EDGE('',*,*,#7466,.F.);
#10804=ORIENTED_EDGE('',*,*,#7465,.T.);
#10805=ORIENTED_EDGE('',*,*,#7467,.T.);
#10806=ORIENTED_EDGE('',*,*,#7468,.F.);
#10807=ORIENTED_EDGE('',*,*,#7467,.F.);
#10808=ORIENTED_EDGE('',*,*,#7464,.T.);
#10809=ORIENTED_EDGE('',*,*,#7469,.T.);
#10810=ORIENTED_EDGE('',*,*,#7470,.F.);
#10811=ORIENTED_EDGE('',*,*,#7469,.F.);
#10812=ORIENTED_EDGE('',*,*,#7463,.F.);
#10813=ORIENTED_EDGE('',*,*,#7471,.F.);
#10814=ORIENTED_EDGE('',*,*,#7472,.T.);
#10815=ORIENTED_EDGE('',*,*,#7473,.F.);
#10816=ORIENTED_EDGE('',*,*,#7474,.F.);
#10817=ORIENTED_EDGE('',*,*,#7475,.F.);
#10818=ORIENTED_EDGE('',*,*,#7474,.T.);
#10819=ORIENTED_EDGE('',*,*,#7476,.T.);
#10820=ORIENTED_EDGE('',*,*,#7477,.F.);
#10821=ORIENTED_EDGE('',*,*,#7476,.F.);
#10822=ORIENTED_EDGE('',*,*,#7473,.T.);
#10823=ORIENTED_EDGE('',*,*,#7478,.T.);
#10824=ORIENTED_EDGE('',*,*,#7479,.F.);
#10825=ORIENTED_EDGE('',*,*,#7478,.F.);
#10826=ORIENTED_EDGE('',*,*,#7472,.F.);
#10827=ORIENTED_EDGE('',*,*,#7480,.F.);
#10828=ORIENTED_EDGE('',*,*,#7481,.T.);
#10829=ORIENTED_EDGE('',*,*,#7482,.F.);
#10830=ORIENTED_EDGE('',*,*,#7483,.F.);
#10831=ORIENTED_EDGE('',*,*,#7484,.F.);
#10832=ORIENTED_EDGE('',*,*,#7483,.T.);
#10833=ORIENTED_EDGE('',*,*,#7485,.T.);
#10834=ORIENTED_EDGE('',*,*,#7486,.F.);
#10835=ORIENTED_EDGE('',*,*,#7485,.F.);
#10836=ORIENTED_EDGE('',*,*,#7482,.T.);
#10837=ORIENTED_EDGE('',*,*,#7487,.T.);
#10838=ORIENTED_EDGE('',*,*,#7488,.F.);
#10839=ORIENTED_EDGE('',*,*,#7487,.F.);
#10840=ORIENTED_EDGE('',*,*,#7481,.F.);
#10841=ORIENTED_EDGE('',*,*,#7489,.F.);
#10842=ORIENTED_EDGE('',*,*,#7490,.T.);
#10843=ORIENTED_EDGE('',*,*,#7491,.F.);
#10844=ORIENTED_EDGE('',*,*,#7492,.F.);
#10845=ORIENTED_EDGE('',*,*,#7493,.F.);
#10846=ORIENTED_EDGE('',*,*,#7492,.T.);
#10847=ORIENTED_EDGE('',*,*,#7494,.T.);
#10848=ORIENTED_EDGE('',*,*,#7495,.F.);
#10849=ORIENTED_EDGE('',*,*,#7494,.F.);
#10850=ORIENTED_EDGE('',*,*,#7491,.T.);
#10851=ORIENTED_EDGE('',*,*,#7496,.T.);
#10852=ORIENTED_EDGE('',*,*,#7497,.F.);
#10853=ORIENTED_EDGE('',*,*,#7496,.F.);
#10854=ORIENTED_EDGE('',*,*,#7490,.F.);
#10855=ORIENTED_EDGE('',*,*,#7498,.F.);
#10856=ORIENTED_EDGE('',*,*,#7499,.T.);
#10857=ORIENTED_EDGE('',*,*,#7500,.F.);
#10858=ORIENTED_EDGE('',*,*,#7501,.F.);
#10859=ORIENTED_EDGE('',*,*,#7502,.F.);
#10860=ORIENTED_EDGE('',*,*,#7501,.T.);
#10861=ORIENTED_EDGE('',*,*,#7503,.T.);
#10862=ORIENTED_EDGE('',*,*,#7504,.F.);
#10863=ORIENTED_EDGE('',*,*,#7503,.F.);
#10864=ORIENTED_EDGE('',*,*,#7500,.T.);
#10865=ORIENTED_EDGE('',*,*,#7505,.T.);
#10866=ORIENTED_EDGE('',*,*,#7506,.F.);
#10867=ORIENTED_EDGE('',*,*,#7505,.F.);
#10868=ORIENTED_EDGE('',*,*,#7499,.F.);
#10869=ORIENTED_EDGE('',*,*,#7507,.F.);
#10870=ORIENTED_EDGE('',*,*,#7508,.T.);
#10871=ORIENTED_EDGE('',*,*,#7509,.T.);
#10872=ORIENTED_EDGE('',*,*,#7510,.F.);
#10873=ORIENTED_EDGE('',*,*,#7511,.T.);
#10874=ORIENTED_EDGE('',*,*,#7512,.F.);
#10875=ORIENTED_EDGE('',*,*,#7508,.F.);
#10876=ORIENTED_EDGE('',*,*,#7513,.F.);
#10877=ORIENTED_EDGE('',*,*,#7509,.F.);
#10878=ORIENTED_EDGE('',*,*,#7512,.T.);
#10879=ORIENTED_EDGE('',*,*,#7514,.T.);
#10880=ORIENTED_EDGE('',*,*,#7515,.F.);
#10881=ORIENTED_EDGE('',*,*,#7514,.F.);
#10882=ORIENTED_EDGE('',*,*,#7511,.F.);
#10883=ORIENTED_EDGE('',*,*,#7516,.F.);
#10884=ORIENTED_EDGE('',*,*,#7517,.T.);
#10885=ORIENTED_EDGE('',*,*,#7518,.F.);
#10886=ORIENTED_EDGE('',*,*,#7519,.F.);
#10887=ORIENTED_EDGE('',*,*,#7520,.F.);
#10888=ORIENTED_EDGE('',*,*,#7519,.T.);
#10889=ORIENTED_EDGE('',*,*,#7521,.T.);
#10890=ORIENTED_EDGE('',*,*,#7522,.F.);
#10891=ORIENTED_EDGE('',*,*,#7521,.F.);
#10892=ORIENTED_EDGE('',*,*,#7518,.T.);
#10893=ORIENTED_EDGE('',*,*,#7523,.T.);
#10894=ORIENTED_EDGE('',*,*,#7524,.F.);
#10895=ORIENTED_EDGE('',*,*,#7523,.F.);
#10896=ORIENTED_EDGE('',*,*,#7517,.F.);
#10897=ORIENTED_EDGE('',*,*,#7525,.F.);
#10898=ORIENTED_EDGE('',*,*,#7526,.T.);
#10899=ORIENTED_EDGE('',*,*,#7527,.F.);
#10900=ORIENTED_EDGE('',*,*,#7528,.F.);
#10901=ORIENTED_EDGE('',*,*,#7529,.F.);
#10902=ORIENTED_EDGE('',*,*,#7528,.T.);
#10903=ORIENTED_EDGE('',*,*,#7530,.T.);
#10904=ORIENTED_EDGE('',*,*,#7531,.F.);
#10905=ORIENTED_EDGE('',*,*,#7530,.F.);
#10906=ORIENTED_EDGE('',*,*,#7527,.T.);
#10907=ORIENTED_EDGE('',*,*,#7532,.T.);
#10908=ORIENTED_EDGE('',*,*,#7533,.F.);
#10909=ORIENTED_EDGE('',*,*,#7532,.F.);
#10910=ORIENTED_EDGE('',*,*,#7526,.F.);
#10911=ORIENTED_EDGE('',*,*,#7534,.F.);
#10912=ORIENTED_EDGE('',*,*,#7535,.T.);
#10913=ORIENTED_EDGE('',*,*,#7536,.F.);
#10914=ORIENTED_EDGE('',*,*,#7537,.F.);
#10915=ORIENTED_EDGE('',*,*,#7538,.F.);
#10916=ORIENTED_EDGE('',*,*,#7537,.T.);
#10917=ORIENTED_EDGE('',*,*,#7539,.T.);
#10918=ORIENTED_EDGE('',*,*,#7540,.F.);
#10919=ORIENTED_EDGE('',*,*,#7539,.F.);
#10920=ORIENTED_EDGE('',*,*,#7536,.T.);
#10921=ORIENTED_EDGE('',*,*,#7541,.T.);
#10922=ORIENTED_EDGE('',*,*,#7542,.F.);
#10923=ORIENTED_EDGE('',*,*,#7541,.F.);
#10924=ORIENTED_EDGE('',*,*,#7535,.F.);
#10925=ORIENTED_EDGE('',*,*,#7543,.F.);
#10926=ORIENTED_EDGE('',*,*,#7544,.T.);
#10927=ORIENTED_EDGE('',*,*,#7545,.F.);
#10928=ORIENTED_EDGE('',*,*,#7546,.F.);
#10929=ORIENTED_EDGE('',*,*,#7547,.F.);
#10930=ORIENTED_EDGE('',*,*,#7546,.T.);
#10931=ORIENTED_EDGE('',*,*,#7548,.T.);
#10932=ORIENTED_EDGE('',*,*,#7549,.F.);
#10933=ORIENTED_EDGE('',*,*,#7548,.F.);
#10934=ORIENTED_EDGE('',*,*,#7545,.T.);
#10935=ORIENTED_EDGE('',*,*,#7550,.T.);
#10936=ORIENTED_EDGE('',*,*,#7551,.F.);
#10937=ORIENTED_EDGE('',*,*,#7550,.F.);
#10938=ORIENTED_EDGE('',*,*,#7544,.F.);
#10939=ORIENTED_EDGE('',*,*,#7552,.F.);
#10940=ORIENTED_EDGE('',*,*,#7553,.T.);
#10941=ORIENTED_EDGE('',*,*,#7554,.F.);
#10942=ORIENTED_EDGE('',*,*,#7555,.F.);
#10943=ORIENTED_EDGE('',*,*,#7556,.F.);
#10944=ORIENTED_EDGE('',*,*,#7555,.T.);
#10945=ORIENTED_EDGE('',*,*,#7557,.T.);
#10946=ORIENTED_EDGE('',*,*,#7558,.F.);
#10947=ORIENTED_EDGE('',*,*,#7557,.F.);
#10948=ORIENTED_EDGE('',*,*,#7554,.T.);
#10949=ORIENTED_EDGE('',*,*,#7559,.T.);
#10950=ORIENTED_EDGE('',*,*,#7560,.F.);
#10951=ORIENTED_EDGE('',*,*,#7559,.F.);
#10952=ORIENTED_EDGE('',*,*,#7553,.F.);
#10953=ORIENTED_EDGE('',*,*,#7561,.F.);
#10954=ORIENTED_EDGE('',*,*,#7562,.T.);
#10955=ORIENTED_EDGE('',*,*,#7563,.F.);
#10956=ORIENTED_EDGE('',*,*,#7564,.F.);
#10957=ORIENTED_EDGE('',*,*,#7565,.F.);
#10958=ORIENTED_EDGE('',*,*,#7564,.T.);
#10959=ORIENTED_EDGE('',*,*,#7566,.T.);
#10960=ORIENTED_EDGE('',*,*,#7567,.F.);
#10961=ORIENTED_EDGE('',*,*,#7566,.F.);
#10962=ORIENTED_EDGE('',*,*,#7563,.T.);
#10963=ORIENTED_EDGE('',*,*,#7568,.T.);
#10964=ORIENTED_EDGE('',*,*,#7569,.F.);
#10965=ORIENTED_EDGE('',*,*,#7568,.F.);
#10966=ORIENTED_EDGE('',*,*,#7562,.F.);
#10967=ORIENTED_EDGE('',*,*,#7570,.F.);
#10968=ORIENTED_EDGE('',*,*,#7571,.T.);
#10969=ORIENTED_EDGE('',*,*,#7572,.F.);
#10970=ORIENTED_EDGE('',*,*,#7573,.F.);
#10971=ORIENTED_EDGE('',*,*,#7574,.F.);
#10972=ORIENTED_EDGE('',*,*,#7573,.T.);
#10973=ORIENTED_EDGE('',*,*,#7575,.T.);
#10974=ORIENTED_EDGE('',*,*,#7576,.F.);
#10975=ORIENTED_EDGE('',*,*,#7575,.F.);
#10976=ORIENTED_EDGE('',*,*,#7572,.T.);
#10977=ORIENTED_EDGE('',*,*,#7577,.T.);
#10978=ORIENTED_EDGE('',*,*,#7578,.F.);
#10979=ORIENTED_EDGE('',*,*,#7577,.F.);
#10980=ORIENTED_EDGE('',*,*,#7571,.F.);
#10981=ORIENTED_EDGE('',*,*,#7579,.F.);
#10982=ORIENTED_EDGE('',*,*,#7580,.T.);
#10983=ORIENTED_EDGE('',*,*,#7581,.F.);
#10984=ORIENTED_EDGE('',*,*,#7582,.F.);
#10985=ORIENTED_EDGE('',*,*,#7583,.F.);
#10986=ORIENTED_EDGE('',*,*,#7582,.T.);
#10987=ORIENTED_EDGE('',*,*,#7584,.T.);
#10988=ORIENTED_EDGE('',*,*,#7585,.F.);
#10989=ORIENTED_EDGE('',*,*,#7584,.F.);
#10990=ORIENTED_EDGE('',*,*,#7581,.T.);
#10991=ORIENTED_EDGE('',*,*,#7586,.T.);
#10992=ORIENTED_EDGE('',*,*,#7587,.F.);
#10993=ORIENTED_EDGE('',*,*,#7586,.F.);
#10994=ORIENTED_EDGE('',*,*,#7580,.F.);
#10995=ORIENTED_EDGE('',*,*,#7588,.F.);
#10996=ORIENTED_EDGE('',*,*,#7589,.T.);
#10997=ORIENTED_EDGE('',*,*,#7590,.F.);
#10998=ORIENTED_EDGE('',*,*,#7591,.F.);
#10999=ORIENTED_EDGE('',*,*,#7592,.F.);
#11000=ORIENTED_EDGE('',*,*,#7591,.T.);
#11001=ORIENTED_EDGE('',*,*,#7593,.T.);
#11002=ORIENTED_EDGE('',*,*,#7594,.F.);
#11003=ORIENTED_EDGE('',*,*,#7593,.F.);
#11004=ORIENTED_EDGE('',*,*,#7590,.T.);
#11005=ORIENTED_EDGE('',*,*,#7595,.T.);
#11006=ORIENTED_EDGE('',*,*,#7596,.F.);
#11007=ORIENTED_EDGE('',*,*,#7595,.F.);
#11008=ORIENTED_EDGE('',*,*,#7589,.F.);
#11009=ORIENTED_EDGE('',*,*,#7597,.T.);
#11010=ORIENTED_EDGE('',*,*,#7598,.T.);
#11011=ORIENTED_EDGE('',*,*,#7599,.T.);
#11012=ORIENTED_EDGE('',*,*,#7598,.F.);
#11013=ORIENTED_EDGE('',*,*,#7597,.F.);
#11014=ORIENTED_EDGE('',*,*,#7600,.T.);
#11015=ORIENTED_EDGE('',*,*,#7601,.T.);
#11016=ORIENTED_EDGE('',*,*,#7600,.F.);
#11017=ORIENTED_EDGE('',*,*,#7602,.F.);
#11018=ORIENTED_EDGE('',*,*,#7599,.F.);
#11019=ORIENTED_EDGE('',*,*,#7603,.F.);
#11020=ORIENTED_EDGE('',*,*,#7244,.F.);
#11021=ORIENTED_EDGE('',*,*,#7096,.F.);
#11022=ORIENTED_EDGE('',*,*,#7245,.F.);
#11023=ORIENTED_EDGE('',*,*,#7604,.T.);
#11024=ORIENTED_EDGE('',*,*,#7603,.T.);
#11025=ORIENTED_EDGE('',*,*,#7604,.F.);
#11026=ORIENTED_EDGE('',*,*,#7164,.T.);
#11027=ORIENTED_EDGE('',*,*,#7241,.T.);
#11028=ORIENTED_EDGE('',*,*,#7605,.F.);
#11029=ORIENTED_EDGE('',*,*,#7250,.T.);
#11030=ORIENTED_EDGE('',*,*,#7601,.F.);
#11031=ORIENTED_EDGE('',*,*,#7605,.T.);
#11032=ORIENTED_EDGE('',*,*,#7240,.T.);
#11033=ORIENTED_EDGE('',*,*,#7172,.T.);
#11034=ORIENTED_EDGE('',*,*,#7169,.T.);
#11035=ORIENTED_EDGE('',*,*,#7249,.T.);
#11036=ORIENTED_EDGE('',*,*,#7606,.F.);
#11037=ORIENTED_EDGE('',*,*,#7607,.T.);
#11038=ORIENTED_EDGE('',*,*,#7602,.T.);
#11039=ORIENTED_EDGE('',*,*,#7607,.F.);
#11040=ORIENTED_EDGE('',*,*,#7271,.T.);
#11041=ORIENTED_EDGE('',*,*,#7608,.F.);
#11042=ORIENTED_EDGE('',*,*,#7585,.T.);
#11043=ORIENTED_EDGE('',*,*,#7587,.T.);
#11044=ORIENTED_EDGE('',*,*,#7579,.T.);
#11045=ORIENTED_EDGE('',*,*,#7609,.F.);
#11046=ORIENTED_EDGE('',*,*,#7286,.T.);
#11047=ORIENTED_EDGE('',*,*,#7288,.T.);
#11048=ORIENTED_EDGE('',*,*,#7280,.T.);
#11049=ORIENTED_EDGE('',*,*,#7610,.F.);
#11050=ORIENTED_EDGE('',*,*,#7576,.T.);
#11051=ORIENTED_EDGE('',*,*,#7578,.T.);
#11052=ORIENTED_EDGE('',*,*,#7570,.T.);
#11053=ORIENTED_EDGE('',*,*,#7611,.F.);
#11054=ORIENTED_EDGE('',*,*,#7295,.T.);
#11055=ORIENTED_EDGE('',*,*,#7297,.T.);
#11056=ORIENTED_EDGE('',*,*,#7289,.T.);
#11057=ORIENTED_EDGE('',*,*,#7612,.F.);
#11058=ORIENTED_EDGE('',*,*,#7567,.T.);
#11059=ORIENTED_EDGE('',*,*,#7569,.T.);
#11060=ORIENTED_EDGE('',*,*,#7561,.T.);
#11061=ORIENTED_EDGE('',*,*,#7613,.F.);
#11062=ORIENTED_EDGE('',*,*,#7304,.T.);
#11063=ORIENTED_EDGE('',*,*,#7306,.T.);
#11064=ORIENTED_EDGE('',*,*,#7298,.T.);
#11065=ORIENTED_EDGE('',*,*,#7614,.F.);
#11066=ORIENTED_EDGE('',*,*,#7558,.T.);
#11067=ORIENTED_EDGE('',*,*,#7560,.T.);
#11068=ORIENTED_EDGE('',*,*,#7552,.T.);
#11069=ORIENTED_EDGE('',*,*,#7615,.F.);
#11070=ORIENTED_EDGE('',*,*,#7313,.T.);
#11071=ORIENTED_EDGE('',*,*,#7315,.T.);
#11072=ORIENTED_EDGE('',*,*,#7307,.T.);
#11073=ORIENTED_EDGE('',*,*,#7616,.F.);
#11074=ORIENTED_EDGE('',*,*,#7549,.T.);
#11075=ORIENTED_EDGE('',*,*,#7551,.T.);
#11076=ORIENTED_EDGE('',*,*,#7543,.T.);
#11077=ORIENTED_EDGE('',*,*,#7617,.F.);
#11078=ORIENTED_EDGE('',*,*,#7322,.T.);
#11079=ORIENTED_EDGE('',*,*,#7324,.T.);
#11080=ORIENTED_EDGE('',*,*,#7316,.T.);
#11081=ORIENTED_EDGE('',*,*,#7618,.F.);
#11082=ORIENTED_EDGE('',*,*,#7540,.T.);
#11083=ORIENTED_EDGE('',*,*,#7542,.T.);
#11084=ORIENTED_EDGE('',*,*,#7534,.T.);
#11085=ORIENTED_EDGE('',*,*,#7619,.F.);
#11086=ORIENTED_EDGE('',*,*,#7331,.T.);
#11087=ORIENTED_EDGE('',*,*,#7333,.T.);
#11088=ORIENTED_EDGE('',*,*,#7325,.T.);
#11089=ORIENTED_EDGE('',*,*,#7620,.F.);
#11090=ORIENTED_EDGE('',*,*,#7531,.T.);
#11091=ORIENTED_EDGE('',*,*,#7533,.T.);
#11092=ORIENTED_EDGE('',*,*,#7525,.T.);
#11093=ORIENTED_EDGE('',*,*,#7621,.F.);
#11094=ORIENTED_EDGE('',*,*,#7340,.T.);
#11095=ORIENTED_EDGE('',*,*,#7342,.T.);
#11096=ORIENTED_EDGE('',*,*,#7334,.T.);
#11097=ORIENTED_EDGE('',*,*,#7622,.F.);
#11098=ORIENTED_EDGE('',*,*,#7522,.T.);
#11099=ORIENTED_EDGE('',*,*,#7524,.T.);
#11100=ORIENTED_EDGE('',*,*,#7516,.T.);
#11101=ORIENTED_EDGE('',*,*,#7623,.F.);
#11102=ORIENTED_EDGE('',*,*,#7350,.T.);
#11103=ORIENTED_EDGE('',*,*,#7352,.T.);
#11104=ORIENTED_EDGE('',*,*,#7624,.T.);
#11105=ORIENTED_EDGE('',*,*,#7606,.T.);
#11106=ORIENTED_EDGE('',*,*,#7624,.F.);
#11107=ORIENTED_EDGE('',*,*,#7353,.T.);
#11108=ORIENTED_EDGE('',*,*,#7343,.T.);
#11109=ORIENTED_EDGE('',*,*,#7625,.F.);
#11110=ORIENTED_EDGE('',*,*,#7360,.T.);
#11111=ORIENTED_EDGE('',*,*,#7362,.T.);
#11112=ORIENTED_EDGE('',*,*,#7354,.T.);
#11113=ORIENTED_EDGE('',*,*,#7626,.F.);
#11114=ORIENTED_EDGE('',*,*,#7504,.T.);
#11115=ORIENTED_EDGE('',*,*,#7506,.T.);
#11116=ORIENTED_EDGE('',*,*,#7498,.T.);
#11117=ORIENTED_EDGE('',*,*,#7627,.F.);
#11118=ORIENTED_EDGE('',*,*,#7369,.T.);
#11119=ORIENTED_EDGE('',*,*,#7371,.T.);
#11120=ORIENTED_EDGE('',*,*,#7363,.T.);
#11121=ORIENTED_EDGE('',*,*,#7628,.F.);
#11122=ORIENTED_EDGE('',*,*,#7495,.T.);
#11123=ORIENTED_EDGE('',*,*,#7497,.T.);
#11124=ORIENTED_EDGE('',*,*,#7489,.T.);
#11125=ORIENTED_EDGE('',*,*,#7629,.F.);
#11126=ORIENTED_EDGE('',*,*,#7378,.T.);
#11127=ORIENTED_EDGE('',*,*,#7380,.T.);
#11128=ORIENTED_EDGE('',*,*,#7372,.T.);
#11129=ORIENTED_EDGE('',*,*,#7630,.F.);
#11130=ORIENTED_EDGE('',*,*,#7486,.T.);
#11131=ORIENTED_EDGE('',*,*,#7488,.T.);
#11132=ORIENTED_EDGE('',*,*,#7480,.T.);
#11133=ORIENTED_EDGE('',*,*,#7631,.F.);
#11134=ORIENTED_EDGE('',*,*,#7387,.T.);
#11135=ORIENTED_EDGE('',*,*,#7389,.T.);
#11136=ORIENTED_EDGE('',*,*,#7381,.T.);
#11137=ORIENTED_EDGE('',*,*,#7632,.F.);
#11138=ORIENTED_EDGE('',*,*,#7477,.T.);
#11139=ORIENTED_EDGE('',*,*,#7479,.T.);
#11140=ORIENTED_EDGE('',*,*,#7471,.T.);
#11141=ORIENTED_EDGE('',*,*,#7633,.F.);
#11142=ORIENTED_EDGE('',*,*,#7396,.T.);
#11143=ORIENTED_EDGE('',*,*,#7398,.T.);
#11144=ORIENTED_EDGE('',*,*,#7390,.T.);
#11145=ORIENTED_EDGE('',*,*,#7634,.F.);
#11146=ORIENTED_EDGE('',*,*,#7468,.T.);
#11147=ORIENTED_EDGE('',*,*,#7470,.T.);
#11148=ORIENTED_EDGE('',*,*,#7462,.T.);
#11149=ORIENTED_EDGE('',*,*,#7635,.F.);
#11150=ORIENTED_EDGE('',*,*,#7405,.T.);
#11151=ORIENTED_EDGE('',*,*,#7407,.T.);
#11152=ORIENTED_EDGE('',*,*,#7399,.T.);
#11153=ORIENTED_EDGE('',*,*,#7636,.F.);
#11154=ORIENTED_EDGE('',*,*,#7459,.T.);
#11155=ORIENTED_EDGE('',*,*,#7461,.T.);
#11156=ORIENTED_EDGE('',*,*,#7453,.T.);
#11157=ORIENTED_EDGE('',*,*,#7637,.F.);
#11158=ORIENTED_EDGE('',*,*,#7414,.T.);
#11159=ORIENTED_EDGE('',*,*,#7416,.T.);
#11160=ORIENTED_EDGE('',*,*,#7408,.T.);
#11161=ORIENTED_EDGE('',*,*,#7638,.F.);
#11162=ORIENTED_EDGE('',*,*,#7450,.T.);
#11163=ORIENTED_EDGE('',*,*,#7452,.T.);
#11164=ORIENTED_EDGE('',*,*,#7444,.T.);
#11165=ORIENTED_EDGE('',*,*,#7639,.F.);
#11166=ORIENTED_EDGE('',*,*,#7423,.T.);
#11167=ORIENTED_EDGE('',*,*,#7425,.T.);
#11168=ORIENTED_EDGE('',*,*,#7417,.T.);
#11169=ORIENTED_EDGE('',*,*,#7640,.F.);
#11170=ORIENTED_EDGE('',*,*,#7441,.T.);
#11171=ORIENTED_EDGE('',*,*,#7443,.T.);
#11172=ORIENTED_EDGE('',*,*,#7435,.T.);
#11173=ORIENTED_EDGE('',*,*,#7641,.F.);
#11174=ORIENTED_EDGE('',*,*,#7432,.T.);
#11175=ORIENTED_EDGE('',*,*,#7434,.T.);
#11176=ORIENTED_EDGE('',*,*,#7426,.T.);
#11177=ORIENTED_EDGE('',*,*,#7642,.F.);
#11178=ORIENTED_EDGE('',*,*,#7513,.T.);
#11179=ORIENTED_EDGE('',*,*,#7515,.T.);
#11180=ORIENTED_EDGE('',*,*,#7510,.T.);
#11181=ORIENTED_EDGE('',*,*,#7643,.F.);
#11182=ORIENTED_EDGE('',*,*,#7594,.T.);
#11183=ORIENTED_EDGE('',*,*,#7596,.T.);
#11184=ORIENTED_EDGE('',*,*,#7588,.T.);
#11185=ORIENTED_EDGE('',*,*,#7644,.F.);
#11186=ORIENTED_EDGE('',*,*,#7277,.T.);
#11187=ORIENTED_EDGE('',*,*,#7279,.T.);
#11188=ORIENTED_EDGE('',*,*,#7645,.F.);
#11189=ORIENTED_EDGE('',*,*,#7646,.T.);
#11190=ORIENTED_EDGE('',*,*,#7349,.T.);
#11191=ORIENTED_EDGE('',*,*,#7623,.T.);
#11192=ORIENTED_EDGE('',*,*,#7520,.T.);
#11193=ORIENTED_EDGE('',*,*,#7622,.T.);
#11194=ORIENTED_EDGE('',*,*,#7338,.T.);
#11195=ORIENTED_EDGE('',*,*,#7621,.T.);
#11196=ORIENTED_EDGE('',*,*,#7529,.T.);
#11197=ORIENTED_EDGE('',*,*,#7620,.T.);
#11198=ORIENTED_EDGE('',*,*,#7329,.T.);
#11199=ORIENTED_EDGE('',*,*,#7619,.T.);
#11200=ORIENTED_EDGE('',*,*,#7538,.T.);
#11201=ORIENTED_EDGE('',*,*,#7618,.T.);
#11202=ORIENTED_EDGE('',*,*,#7320,.T.);
#11203=ORIENTED_EDGE('',*,*,#7617,.T.);
#11204=ORIENTED_EDGE('',*,*,#7547,.T.);
#11205=ORIENTED_EDGE('',*,*,#7616,.T.);
#11206=ORIENTED_EDGE('',*,*,#7311,.T.);
#11207=ORIENTED_EDGE('',*,*,#7615,.T.);
#11208=ORIENTED_EDGE('',*,*,#7556,.T.);
#11209=ORIENTED_EDGE('',*,*,#7614,.T.);
#11210=ORIENTED_EDGE('',*,*,#7302,.T.);
#11211=ORIENTED_EDGE('',*,*,#7613,.T.);
#11212=ORIENTED_EDGE('',*,*,#7565,.T.);
#11213=ORIENTED_EDGE('',*,*,#7612,.T.);
#11214=ORIENTED_EDGE('',*,*,#7293,.T.);
#11215=ORIENTED_EDGE('',*,*,#7611,.T.);
#11216=ORIENTED_EDGE('',*,*,#7574,.T.);
#11217=ORIENTED_EDGE('',*,*,#7610,.T.);
#11218=ORIENTED_EDGE('',*,*,#7284,.T.);
#11219=ORIENTED_EDGE('',*,*,#7609,.T.);
#11220=ORIENTED_EDGE('',*,*,#7583,.T.);
#11221=ORIENTED_EDGE('',*,*,#7608,.T.);
#11222=ORIENTED_EDGE('',*,*,#7275,.T.);
#11223=ORIENTED_EDGE('',*,*,#7644,.T.);
#11224=ORIENTED_EDGE('',*,*,#7592,.T.);
#11225=ORIENTED_EDGE('',*,*,#7643,.T.);
#11226=ORIENTED_EDGE('',*,*,#7507,.T.);
#11227=ORIENTED_EDGE('',*,*,#7642,.T.);
#11228=ORIENTED_EDGE('',*,*,#7430,.T.);
#11229=ORIENTED_EDGE('',*,*,#7641,.T.);
#11230=ORIENTED_EDGE('',*,*,#7439,.T.);
#11231=ORIENTED_EDGE('',*,*,#7640,.T.);
#11232=ORIENTED_EDGE('',*,*,#7421,.T.);
#11233=ORIENTED_EDGE('',*,*,#7639,.T.);
#11234=ORIENTED_EDGE('',*,*,#7448,.T.);
#11235=ORIENTED_EDGE('',*,*,#7638,.T.);
#11236=ORIENTED_EDGE('',*,*,#7412,.T.);
#11237=ORIENTED_EDGE('',*,*,#7637,.T.);
#11238=ORIENTED_EDGE('',*,*,#7457,.T.);
#11239=ORIENTED_EDGE('',*,*,#7636,.T.);
#11240=ORIENTED_EDGE('',*,*,#7403,.T.);
#11241=ORIENTED_EDGE('',*,*,#7635,.T.);
#11242=ORIENTED_EDGE('',*,*,#7466,.T.);
#11243=ORIENTED_EDGE('',*,*,#7634,.T.);
#11244=ORIENTED_EDGE('',*,*,#7394,.T.);
#11245=ORIENTED_EDGE('',*,*,#7633,.T.);
#11246=ORIENTED_EDGE('',*,*,#7475,.T.);
#11247=ORIENTED_EDGE('',*,*,#7632,.T.);
#11248=ORIENTED_EDGE('',*,*,#7385,.T.);
#11249=ORIENTED_EDGE('',*,*,#7631,.T.);
#11250=ORIENTED_EDGE('',*,*,#7484,.T.);
#11251=ORIENTED_EDGE('',*,*,#7630,.T.);
#11252=ORIENTED_EDGE('',*,*,#7376,.T.);
#11253=ORIENTED_EDGE('',*,*,#7629,.T.);
#11254=ORIENTED_EDGE('',*,*,#7493,.T.);
#11255=ORIENTED_EDGE('',*,*,#7628,.T.);
#11256=ORIENTED_EDGE('',*,*,#7367,.T.);
#11257=ORIENTED_EDGE('',*,*,#7627,.T.);
#11258=ORIENTED_EDGE('',*,*,#7502,.T.);
#11259=ORIENTED_EDGE('',*,*,#7626,.T.);
#11260=ORIENTED_EDGE('',*,*,#7358,.T.);
#11261=ORIENTED_EDGE('',*,*,#7625,.T.);
#11262=ORIENTED_EDGE('',*,*,#7347,.T.);
#11263=ORIENTED_EDGE('',*,*,#7646,.F.);
#11264=ORIENTED_EDGE('',*,*,#7645,.T.);
#11265=ORIENTED_EDGE('',*,*,#7253,.T.);
#11266=ORIENTED_EDGE('',*,*,#7269,.T.);
#11267=ORIENTED_EDGE('',*,*,#7266,.T.);
#11268=ORIENTED_EDGE('',*,*,#7263,.T.);
#11269=ORIENTED_EDGE('',*,*,#7260,.T.);
#11270=ORIENTED_EDGE('',*,*,#7257,.T.);
#11271=ORIENTED_EDGE('',*,*,#7647,.T.);
#11272=ORIENTED_EDGE('',*,*,#7648,.T.);
#11273=ORIENTED_EDGE('',*,*,#7649,.T.);
#11274=ORIENTED_EDGE('',*,*,#7650,.T.);
#11275=ORIENTED_EDGE('',*,*,#7648,.F.);
#11276=ORIENTED_EDGE('',*,*,#7647,.F.);
#11277=ORIENTED_EDGE('',*,*,#7651,.F.);
#11278=ORIENTED_EDGE('',*,*,#7649,.F.);
#11279=ORIENTED_EDGE('',*,*,#7650,.F.);
#11280=ORIENTED_EDGE('',*,*,#7652,.T.);
#11281=ORIENTED_EDGE('',*,*,#7653,.T.);
#11282=ORIENTED_EDGE('',*,*,#7652,.F.);
#11283=ORIENTED_EDGE('',*,*,#7654,.T.);
#11284=ORIENTED_EDGE('',*,*,#7655,.T.);
#11285=ORIENTED_EDGE('',*,*,#7656,.T.);
#11286=ORIENTED_EDGE('',*,*,#7657,.T.);
#11287=ORIENTED_EDGE('',*,*,#7655,.F.);
#11288=ORIENTED_EDGE('',*,*,#7658,.F.);
#11289=ORIENTED_EDGE('',*,*,#7659,.F.);
#11290=ORIENTED_EDGE('',*,*,#7660,.T.);
#11291=ORIENTED_EDGE('',*,*,#7656,.F.);
#11292=ORIENTED_EDGE('',*,*,#7657,.F.);
#11293=ORIENTED_EDGE('',*,*,#7660,.F.);
#11294=ORIENTED_EDGE('',*,*,#7661,.F.);
#11295=ORIENTED_EDGE('',*,*,#7654,.F.);
#11296=ORIENTED_EDGE('',*,*,#7658,.T.);
#11297=ORIENTED_EDGE('',*,*,#7659,.T.);
#11298=ORIENTED_EDGE('',*,*,#7662,.T.);
#11299=ORIENTED_EDGE('',*,*,#7651,.T.);
#11300=ORIENTED_EDGE('',*,*,#7662,.F.);
#11301=ORIENTED_EDGE('',*,*,#7653,.F.);
#11302=ORIENTED_EDGE('',*,*,#7663,.T.);
#11303=ORIENTED_EDGE('',*,*,#7661,.T.);
#11304=ORIENTED_EDGE('',*,*,#7663,.F.);
#11305=ORIENTED_EDGE('',*,*,#7664,.F.);
#11306=ORIENTED_EDGE('',*,*,#7665,.F.);
#11307=ORIENTED_EDGE('',*,*,#7666,.F.);
#11308=ORIENTED_EDGE('',*,*,#7667,.F.);
#11309=ORIENTED_EDGE('',*,*,#7668,.F.);
#11310=ORIENTED_EDGE('',*,*,#7669,.F.);
#11311=ORIENTED_EDGE('',*,*,#7670,.F.);
#11312=ORIENTED_EDGE('',*,*,#7671,.F.);
#11313=ORIENTED_EDGE('',*,*,#7672,.F.);
#11314=ORIENTED_EDGE('',*,*,#7673,.F.);
#11315=ORIENTED_EDGE('',*,*,#7674,.F.);
#11316=ORIENTED_EDGE('',*,*,#7675,.F.);
#11317=ORIENTED_EDGE('',*,*,#7676,.F.);
#11318=ORIENTED_EDGE('',*,*,#7677,.F.);
#11319=ORIENTED_EDGE('',*,*,#7678,.F.);
#11320=ORIENTED_EDGE('',*,*,#7679,.F.);
#11321=ORIENTED_EDGE('',*,*,#7680,.F.);
#11322=ORIENTED_EDGE('',*,*,#7681,.F.);
#11323=ORIENTED_EDGE('',*,*,#7682,.T.);
#11324=ORIENTED_EDGE('',*,*,#7683,.T.);
#11325=ORIENTED_EDGE('',*,*,#7677,.T.);
#11326=ORIENTED_EDGE('',*,*,#7684,.T.);
#11327=ORIENTED_EDGE('',*,*,#7680,.T.);
#11328=ORIENTED_EDGE('',*,*,#7685,.T.);
#11329=ORIENTED_EDGE('',*,*,#7686,.T.);
#11330=ORIENTED_EDGE('',*,*,#7687,.T.);
#11331=ORIENTED_EDGE('',*,*,#7681,.T.);
#11332=ORIENTED_EDGE('',*,*,#7688,.T.);
#11333=ORIENTED_EDGE('',*,*,#7689,.T.);
#11334=ORIENTED_EDGE('',*,*,#7690,.T.);
#11335=ORIENTED_EDGE('',*,*,#7679,.T.);
#11336=ORIENTED_EDGE('',*,*,#7691,.T.);
#11337=ORIENTED_EDGE('',*,*,#7674,.T.);
#11338=ORIENTED_EDGE('',*,*,#7692,.T.);
#11339=ORIENTED_EDGE('',*,*,#7693,.T.);
#11340=ORIENTED_EDGE('',*,*,#7694,.T.);
#11341=ORIENTED_EDGE('',*,*,#7671,.T.);
#11342=ORIENTED_EDGE('',*,*,#7695,.T.);
#11343=ORIENTED_EDGE('',*,*,#7678,.T.);
#11344=ORIENTED_EDGE('',*,*,#7696,.T.);
#11345=ORIENTED_EDGE('',*,*,#7697,.T.);
#11346=ORIENTED_EDGE('',*,*,#7698,.T.);
#11347=ORIENTED_EDGE('',*,*,#7676,.T.);
#11348=ORIENTED_EDGE('',*,*,#7699,.T.);
#11349=ORIENTED_EDGE('',*,*,#7700,.T.);
#11350=ORIENTED_EDGE('',*,*,#7701,.T.);
#11351=ORIENTED_EDGE('',*,*,#7675,.T.);
#11352=ORIENTED_EDGE('',*,*,#7702,.T.);
#11353=ORIENTED_EDGE('',*,*,#7703,.T.);
#11354=ORIENTED_EDGE('',*,*,#7704,.T.);
#11355=ORIENTED_EDGE('',*,*,#7673,.T.);
#11356=ORIENTED_EDGE('',*,*,#7705,.T.);
#11357=ORIENTED_EDGE('',*,*,#7668,.T.);
#11358=ORIENTED_EDGE('',*,*,#7706,.T.);
#11359=ORIENTED_EDGE('',*,*,#7707,.T.);
#11360=ORIENTED_EDGE('',*,*,#7708,.T.);
#11361=ORIENTED_EDGE('',*,*,#7709,.T.);
#11362=ORIENTED_EDGE('',*,*,#7665,.T.);
#11363=ORIENTED_EDGE('',*,*,#7710,.T.);
#11364=ORIENTED_EDGE('',*,*,#7672,.T.);
#11365=ORIENTED_EDGE('',*,*,#7711,.T.);
#11366=ORIENTED_EDGE('',*,*,#7712,.T.);
#11367=ORIENTED_EDGE('',*,*,#7713,.T.);
#11368=ORIENTED_EDGE('',*,*,#7670,.T.);
#11369=ORIENTED_EDGE('',*,*,#7714,.T.);
#11370=ORIENTED_EDGE('',*,*,#7715,.T.);
#11371=ORIENTED_EDGE('',*,*,#7716,.T.);
#11372=ORIENTED_EDGE('',*,*,#7669,.T.);
#11373=ORIENTED_EDGE('',*,*,#7717,.T.);
#11374=ORIENTED_EDGE('',*,*,#7718,.T.);
#11375=ORIENTED_EDGE('',*,*,#7719,.T.);
#11376=ORIENTED_EDGE('',*,*,#7667,.T.);
#11377=ORIENTED_EDGE('',*,*,#7720,.T.);
#11378=ORIENTED_EDGE('',*,*,#7666,.T.);
#11379=ORIENTED_EDGE('',*,*,#7721,.T.);
#11380=ORIENTED_EDGE('',*,*,#7722,.T.);
#11381=ORIENTED_EDGE('',*,*,#7723,.T.);
#11382=ORIENTED_EDGE('',*,*,#7664,.T.);
#11383=ORIENTED_EDGE('',*,*,#7724,.T.);
#11384=ORIENTED_EDGE('',*,*,#7699,.F.);
#11385=ORIENTED_EDGE('',*,*,#7695,.F.);
#11386=ORIENTED_EDGE('',*,*,#7713,.F.);
#11387=ORIENTED_EDGE('',*,*,#7725,.T.);
#11388=ORIENTED_EDGE('',*,*,#7714,.F.);
#11389=ORIENTED_EDGE('',*,*,#7710,.F.);
#11390=ORIENTED_EDGE('',*,*,#7723,.F.);
#11391=ORIENTED_EDGE('',*,*,#7726,.T.);
#11392=ORIENTED_EDGE('',*,*,#7724,.F.);
#11393=ORIENTED_EDGE('',*,*,#7720,.F.);
#11394=ORIENTED_EDGE('',*,*,#7716,.F.);
#11395=ORIENTED_EDGE('',*,*,#7727,.T.);
#11396=ORIENTED_EDGE('',*,*,#7728,.F.);
#11397=ORIENTED_EDGE('',*,*,#7729,.T.);
#11398=ORIENTED_EDGE('',*,*,#7730,.F.);
#11399=ORIENTED_EDGE('',*,*,#7686,.F.);
#11400=ORIENTED_EDGE('',*,*,#7731,.F.);
#11401=ORIENTED_EDGE('',*,*,#7697,.F.);
#11402=ORIENTED_EDGE('',*,*,#7725,.F.);
#11403=ORIENTED_EDGE('',*,*,#7712,.F.);
#11404=ORIENTED_EDGE('',*,*,#7726,.F.);
#11405=ORIENTED_EDGE('',*,*,#7722,.F.);
#11406=ORIENTED_EDGE('',*,*,#7727,.F.);
#11407=ORIENTED_EDGE('',*,*,#7715,.F.);
#11408=ORIENTED_EDGE('',*,*,#7732,.F.);
#11409=ORIENTED_EDGE('',*,*,#7700,.F.);
#11410=ORIENTED_EDGE('',*,*,#7733,.F.);
#11411=ORIENTED_EDGE('',*,*,#7729,.F.);
#11412=ORIENTED_EDGE('',*,*,#7692,.F.);
#11413=ORIENTED_EDGE('',*,*,#7704,.F.);
#11414=ORIENTED_EDGE('',*,*,#7734,.F.);
#11415=ORIENTED_EDGE('',*,*,#7706,.F.);
#11416=ORIENTED_EDGE('',*,*,#7719,.F.);
#11417=ORIENTED_EDGE('',*,*,#7735,.F.);
#11418=ORIENTED_EDGE('',*,*,#7709,.F.);
#11419=ORIENTED_EDGE('',*,*,#7736,.F.);
#11420=ORIENTED_EDGE('',*,*,#7721,.F.);
#11421=ORIENTED_EDGE('',*,*,#7694,.F.);
#11422=ORIENTED_EDGE('',*,*,#7737,.F.);
#11423=ORIENTED_EDGE('',*,*,#7711,.F.);
#11424=ORIENTED_EDGE('',*,*,#7683,.F.);
#11425=ORIENTED_EDGE('',*,*,#7738,.F.);
#11426=ORIENTED_EDGE('',*,*,#7696,.F.);
#11427=ORIENTED_EDGE('',*,*,#7685,.F.);
#11428=ORIENTED_EDGE('',*,*,#7690,.F.);
#11429=ORIENTED_EDGE('',*,*,#7739,.F.);
#11430=ORIENTED_EDGE('',*,*,#7740,.T.);
#11431=ORIENTED_EDGE('',*,*,#7741,.T.);
#11432=ORIENTED_EDGE('',*,*,#7707,.F.);
#11433=ORIENTED_EDGE('',*,*,#7737,.T.);
#11434=ORIENTED_EDGE('',*,*,#7693,.F.);
#11435=ORIENTED_EDGE('',*,*,#7738,.T.);
#11436=ORIENTED_EDGE('',*,*,#7682,.F.);
#11437=ORIENTED_EDGE('',*,*,#7739,.T.);
#11438=ORIENTED_EDGE('',*,*,#7689,.F.);
#11439=ORIENTED_EDGE('',*,*,#7734,.T.);
#11440=ORIENTED_EDGE('',*,*,#7703,.F.);
#11441=ORIENTED_EDGE('',*,*,#7735,.T.);
#11442=ORIENTED_EDGE('',*,*,#7718,.F.);
#11443=ORIENTED_EDGE('',*,*,#7736,.T.);
#11444=ORIENTED_EDGE('',*,*,#7708,.F.);
#11445=ORIENTED_EDGE('',*,*,#7741,.F.);
#11446=ORIENTED_EDGE('',*,*,#7740,.F.);
#11447=ORIENTED_EDGE('',*,*,#7742,.F.);
#11448=ORIENTED_EDGE('',*,*,#7743,.T.);
#11449=ORIENTED_EDGE('',*,*,#7744,.T.);
#11450=ORIENTED_EDGE('',*,*,#7742,.T.);
#11451=ORIENTED_EDGE('',*,*,#7744,.F.);
#11452=ORIENTED_EDGE('',*,*,#7743,.F.);
#11453=ORIENTED_EDGE('',*,*,#7745,.T.);
#11454=ORIENTED_EDGE('',*,*,#7746,.F.);
#11455=ORIENTED_EDGE('',*,*,#7745,.F.);
#11456=ORIENTED_EDGE('',*,*,#7746,.T.);
#11457=ORIENTED_EDGE('',*,*,#7747,.T.);
#11458=ORIENTED_EDGE('',*,*,#7748,.T.);
#11459=ORIENTED_EDGE('',*,*,#7747,.F.);
#11460=ORIENTED_EDGE('',*,*,#7748,.F.);
#11461=ORIENTED_EDGE('',*,*,#7749,.T.);
#11462=ORIENTED_EDGE('',*,*,#7750,.F.);
#11463=ORIENTED_EDGE('',*,*,#7749,.F.);
#11464=ORIENTED_EDGE('',*,*,#7750,.T.);
#11465=ORIENTED_EDGE('',*,*,#7751,.T.);
#11466=ORIENTED_EDGE('',*,*,#7752,.T.);
#11467=ORIENTED_EDGE('',*,*,#7751,.F.);
#11468=ORIENTED_EDGE('',*,*,#7728,.T.);
#11469=ORIENTED_EDGE('',*,*,#7752,.F.);
#11470=ORIENTED_EDGE('',*,*,#7701,.F.);
#11471=ORIENTED_EDGE('',*,*,#7732,.T.);
#11472=ORIENTED_EDGE('',*,*,#7717,.F.);
#11473=ORIENTED_EDGE('',*,*,#7705,.F.);
#11474=ORIENTED_EDGE('',*,*,#7687,.F.);
#11475=ORIENTED_EDGE('',*,*,#7730,.T.);
#11476=ORIENTED_EDGE('',*,*,#7733,.T.);
#11477=ORIENTED_EDGE('',*,*,#7702,.F.);
#11478=ORIENTED_EDGE('',*,*,#7691,.F.);
#11479=ORIENTED_EDGE('',*,*,#7698,.F.);
#11480=ORIENTED_EDGE('',*,*,#7731,.T.);
#11481=ORIENTED_EDGE('',*,*,#7688,.F.);
#11482=ORIENTED_EDGE('',*,*,#7684,.F.);
#11483=PLANE('',#12615);
#11484=PLANE('',#12616);
#11485=PLANE('',#12620);
#11486=PLANE('',#12621);
#11487=PLANE('',#12622);
#11488=PLANE('',#12623);
#11489=PLANE('',#12624);
#11490=PLANE('',#12625);
#11491=PLANE('',#12626);
#11492=PLANE('',#12627);
#11493=PLANE('',#12628);
#11494=PLANE('',#12629);
#11495=PLANE('',#12630);
#11496=PLANE('',#12632);
#11497=PLANE('',#12633);
#11498=PLANE('',#12634);
#11499=PLANE('',#12635);
#11500=PLANE('',#12636);
#11501=PLANE('',#12637);
#11502=PLANE('',#12638);
#11503=PLANE('',#12639);
#11504=PLANE('',#12640);
#11505=PLANE('',#12641);
#11506=PLANE('',#12642);
#11507=PLANE('',#12643);
#11508=PLANE('',#12645);
#11509=PLANE('',#12646);
#11510=PLANE('',#12647);
#11511=PLANE('',#12648);
#11512=PLANE('',#12649);
#11513=PLANE('',#12650);
#11514=PLANE('',#12651);
#11515=PLANE('',#12652);
#11516=PLANE('',#12653);
#11517=PLANE('',#12654);
#11518=PLANE('',#12655);
#11519=PLANE('',#12656);
#11520=PLANE('',#12657);
#11521=PLANE('',#12658);
#11522=PLANE('',#12659);
#11523=PLANE('',#12663);
#11524=PLANE('',#12664);
#11525=PLANE('',#12665);
#11526=PLANE('',#12666);
#11527=PLANE('',#12667);
#11528=PLANE('',#12672);
#11529=PLANE('',#12673);
#11530=PLANE('',#12674);
#11531=PLANE('',#12675);
#11532=PLANE('',#12676);
#11533=PLANE('',#12677);
#11534=PLANE('',#12678);
#11535=PLANE('',#12679);
#11536=PLANE('',#12684);
#11537=PLANE('',#12685);
#11538=PLANE('',#12686);
#11539=PLANE('',#12687);
#11540=PLANE('',#12688);
#11541=PLANE('',#12689);
#11542=PLANE('',#12715);
#11543=PLANE('',#12719);
#11544=PLANE('',#12729);
#11545=PLANE('',#12733);
#11546=PLANE('',#12742);
#11547=PLANE('',#12746);
#11548=PLANE('',#12751);
#11549=PLANE('',#12752);
#11550=PLANE('',#12753);
#11551=PLANE('',#12754);
#11552=PLANE('',#12755);
#11553=PLANE('',#12756);
#11554=PLANE('',#12757);
#11555=PLANE('',#12764);
#11556=PLANE('',#12774);
#11557=PLANE('',#12802);
#11558=PLANE('',#12856);
#11559=PLANE('',#12864);
#11560=PLANE('',#12872);
#11561=PLANE('',#12875);
#11562=PLANE('',#12877);
#11563=PLANE('',#12879);
#11564=PLANE('',#12880);
#11565=PLANE('',#12882);
#11566=PLANE('',#12883);
#11567=PLANE('',#12885);
#11568=PLANE('',#12891);
#11569=PLANE('',#12895);
#11570=PLANE('',#12976);
#11571=PLANE('',#12977);
#11572=PLANE('',#12985);
#11573=PLANE('',#12987);
#11574=PLANE('',#12990);
#11575=PLANE('',#12996);
#11576=PLANE('',#12999);
#11577=PLANE('',#13077);
#11578=PLANE('',#13085);
#11579=PLANE('',#13092);
#11580=PLANE('',#13093);
#11581=PLANE('',#13100);
#11582=PLANE('',#13104);
#11583=PLANE('',#13106);
#11584=PLANE('',#13108);
#11585=PLANE('',#13109);
#11586=PLANE('',#13110);
#11587=PLANE('',#13112);
#11588=PLANE('',#13118);
#11589=PLANE('',#13119);
#11590=PLANE('',#13123);
#11591=PLANE('',#13124);
#11592=PLANE('',#13129);
#11593=PLANE('',#13130);
#11594=PLANE('',#13131);
#11595=PLANE('',#13132);
#11596=PLANE('',#13133);
#11597=PLANE('',#13152);
#11598=PLANE('',#13155);
#11599=PLANE('',#13160);
#11600=PLANE('',#13161);
#11601=PLANE('',#13162);
#11602=PLANE('',#13163);
#11603=PLANE('',#13164);
#11604=PLANE('',#13165);
#11605=PLANE('',#13166);
#11606=PLANE('',#13167);
#11607=PLANE('',#13174);
#11608=PLANE('',#13227);
#11609=PLANE('',#13234);
#11610=PLANE('',#13235);
#11611=PLANE('',#13236);
#11612=PLANE('',#13237);
#11613=PLANE('',#13238);
#11614=PLANE('',#13239);
#11615=PLANE('',#13240);
#11616=PLANE('',#13241);
#11617=PLANE('',#13242);
#11618=PLANE('',#13244);
#11619=PLANE('',#13245);
#11620=PLANE('',#13247);
#11621=PLANE('',#13248);
#11622=PLANE('',#13250);
#11623=PLANE('',#13251);
#11624=PLANE('',#13253);
#11625=PLANE('',#13254);
#11626=PLANE('',#13256);
#11627=PLANE('',#13257);
#11628=PLANE('',#13259);
#11629=PLANE('',#13260);
#11630=PLANE('',#13262);
#11631=PLANE('',#13263);
#11632=PLANE('',#13265);
#11633=PLANE('',#13266);
#11634=PLANE('',#13268);
#11635=PLANE('',#13269);
#11636=PLANE('',#13271);
#11637=PLANE('',#13272);
#11638=PLANE('',#13274);
#11639=PLANE('',#13275);
#11640=PLANE('',#13277);
#11641=PLANE('',#13278);
#11642=PLANE('',#13280);
#11643=PLANE('',#13281);
#11644=PLANE('',#13283);
#11645=PLANE('',#13284);
#11646=PLANE('',#13286);
#11647=PLANE('',#13287);
#11648=PLANE('',#13289);
#11649=PLANE('',#13290);
#11650=PLANE('',#13293);
#11651=PLANE('',#13294);
#11652=PLANE('',#13297);
#11653=PLANE('',#13298);
#11654=PLANE('',#13300);
#11655=PLANE('',#13301);
#11656=PLANE('',#13303);
#11657=PLANE('',#13304);
#11658=PLANE('',#13306);
#11659=PLANE('',#13307);
#11660=PLANE('',#13309);
#11661=PLANE('',#13310);
#11662=PLANE('',#13312);
#11663=PLANE('',#13313);
#11664=PLANE('',#13315);
#11665=PLANE('',#13316);
#11666=PLANE('',#13318);
#11667=PLANE('',#13319);
#11668=PLANE('',#13321);
#11669=PLANE('',#13322);
#11670=PLANE('',#13324);
#11671=PLANE('',#13325);
#11672=PLANE('',#13327);
#11673=PLANE('',#13328);
#11674=PLANE('',#13330);
#11675=PLANE('',#13331);
#11676=PLANE('',#13333);
#11677=PLANE('',#13334);
#11678=PLANE('',#13336);
#11679=PLANE('',#13337);
#11680=PLANE('',#13339);
#11681=PLANE('',#13340);
#11682=PLANE('',#13342);
#11683=PLANE('',#13343);
#11684=PLANE('',#13345);
#11685=PLANE('',#13346);
#11686=PLANE('',#13348);
#11687=PLANE('',#13349);
#11688=PLANE('',#13351);
#11689=PLANE('',#13352);
#11690=PLANE('',#13354);
#11691=PLANE('',#13355);
#11692=PLANE('',#13357);
#11693=PLANE('',#13358);
#11694=PLANE('',#13360);
#11695=PLANE('',#13361);
#11696=PLANE('',#13363);
#11697=PLANE('',#13364);
#11698=PLANE('',#13366);
#11699=PLANE('',#13367);
#11700=PLANE('',#13369);
#11701=PLANE('',#13370);
#11702=PLANE('',#13372);
#11703=PLANE('',#13373);
#11704=PLANE('',#13375);
#11705=PLANE('',#13376);
#11706=PLANE('',#13378);
#11707=PLANE('',#13379);
#11708=PLANE('',#13381);
#11709=PLANE('',#13382);
#11710=PLANE('',#13384);
#11711=PLANE('',#13385);
#11712=PLANE('',#13387);
#11713=PLANE('',#13388);
#11714=PLANE('',#13390);
#11715=PLANE('',#13391);
#11716=PLANE('',#13393);
#11717=PLANE('',#13394);
#11718=PLANE('',#13396);
#11719=PLANE('',#13397);
#11720=PLANE('',#13399);
#11721=PLANE('',#13401);
#11722=PLANE('',#13402);
#11723=PLANE('',#13403);
#11724=PLANE('',#13405);
#11725=PLANE('',#13406);
#11726=PLANE('',#13408);
#11727=PLANE('',#13409);
#11728=PLANE('',#13411);
#11729=PLANE('',#13412);
#11730=PLANE('',#13414);
#11731=PLANE('',#13415);
#11732=PLANE('',#13417);
#11733=PLANE('',#13418);
#11734=PLANE('',#13420);
#11735=PLANE('',#13421);
#11736=PLANE('',#13423);
#11737=PLANE('',#13424);
#11738=PLANE('',#13426);
#11739=PLANE('',#13427);
#11740=PLANE('',#13429);
#11741=PLANE('',#13430);
#11742=PLANE('',#13432);
#11743=PLANE('',#13433);
#11744=PLANE('',#13435);
#11745=PLANE('',#13436);
#11746=PLANE('',#13438);
#11747=PLANE('',#13439);
#11748=PLANE('',#13441);
#11749=PLANE('',#13442);
#11750=PLANE('',#13444);
#11751=PLANE('',#13445);
#11752=PLANE('',#13447);
#11753=PLANE('',#13448);
#11754=PLANE('',#13450);
#11755=PLANE('',#13451);
#11756=PLANE('',#13453);
#11757=PLANE('',#13454);
#11758=PLANE('',#13456);
#11759=PLANE('',#13457);
#11760=PLANE('',#13465);
#11761=PLANE('',#13467);
#11762=PLANE('',#13472);
#11763=PLANE('',#13514);
#11764=PLANE('',#13520);
#11765=PLANE('',#13531);
#11766=PLANE('',#13536);
#11767=PLANE('',#13537);
#11768=PLANE('',#13538);
#11769=PLANE('',#13539);
#11770=PLANE('',#13540);
#11771=PLANE('',#13541);
#11772=PLANE('',#13542);
#11773=PLANE('',#13543);
#11774=PLANE('',#13544);
#11775=PLANE('',#13545);
#11776=PLANE('',#13546);
#11777=PLANE('',#13547);
#11778=PLANE('',#13548);
#11779=PLANE('',#13549);
#11780=PLANE('',#13550);
#11781=PLANE('',#13567);
#11782=PLANE('',#13579);
#11783=PLANE('',#13580);
#11784=PLANE('',#13581);
#11785=PLANE('',#13582);
#11786=ADVANCED_FACE('',(#1819),#11483,.T.);
#11787=ADVANCED_FACE('',(#1820,#1340),#11484,.T.);
#11788=ADVANCED_FACE('',(#1821),#11485,.T.);
#11789=ADVANCED_FACE('',(#1822),#11486,.T.);
#11790=ADVANCED_FACE('',(#1823),#11487,.T.);
#11791=ADVANCED_FACE('',(#1824),#11488,.T.);
#11792=ADVANCED_FACE('',(#1825),#11489,.T.);
#11793=ADVANCED_FACE('',(#1826),#11490,.T.);
#11794=ADVANCED_FACE('',(#1827),#11491,.T.);
#11795=ADVANCED_FACE('',(#1828),#11492,.T.);
#11796=ADVANCED_FACE('',(#1829),#11493,.T.);
#11797=ADVANCED_FACE('',(#1830),#11494,.T.);
#11798=ADVANCED_FACE('',(#1831,#1341),#11495,.T.);
#11799=ADVANCED_FACE('',(#1832),#11496,.T.);
#11800=ADVANCED_FACE('',(#1833),#11497,.T.);
#11801=ADVANCED_FACE('',(#1834),#11498,.T.);
#11802=ADVANCED_FACE('',(#1835),#11499,.T.);
#11803=ADVANCED_FACE('',(#1836),#11500,.T.);
#11804=ADVANCED_FACE('',(#1837),#11501,.T.);
#11805=ADVANCED_FACE('',(#1838),#11502,.T.);
#11806=ADVANCED_FACE('',(#1839),#11503,.T.);
#11807=ADVANCED_FACE('',(#1840),#11504,.T.);
#11808=ADVANCED_FACE('',(#1841),#11505,.T.);
#11809=ADVANCED_FACE('',(#1842),#11506,.T.);
#11810=ADVANCED_FACE('',(#1843,#1342),#11507,.T.);
#11811=ADVANCED_FACE('',(#1844),#11508,.T.);
#11812=ADVANCED_FACE('',(#1845),#11509,.T.);
#11813=ADVANCED_FACE('',(#1846),#11510,.T.);
#11814=ADVANCED_FACE('',(#1847),#11511,.T.);
#11815=ADVANCED_FACE('',(#1848),#11512,.T.);
#11816=ADVANCED_FACE('',(#1849),#11513,.T.);
#11817=ADVANCED_FACE('',(#1850),#11514,.T.);
#11818=ADVANCED_FACE('',(#1851),#11515,.T.);
#11819=ADVANCED_FACE('',(#1852),#11516,.T.);
#11820=ADVANCED_FACE('',(#1853),#11517,.T.);
#11821=ADVANCED_FACE('',(#1854),#11518,.T.);
#11822=ADVANCED_FACE('',(#1855),#11519,.T.);
#11823=ADVANCED_FACE('',(#1856),#11520,.T.);
#11824=ADVANCED_FACE('',(#1857),#11521,.T.);
#11825=ADVANCED_FACE('',(#1858,#1343),#11522,.T.);
#11826=ADVANCED_FACE('',(#1859),#11523,.T.);
#11827=ADVANCED_FACE('',(#1860),#11524,.T.);
#11828=ADVANCED_FACE('',(#1861),#11525,.T.);
#11829=ADVANCED_FACE('',(#1862),#11526,.T.);
#11830=ADVANCED_FACE('',(#1863),#1186,.T.);
#11831=ADVANCED_FACE('',(#1864),#1187,.F.);
#11832=ADVANCED_FACE('',(#1865,#1344,#1345,#1346,#1347),#11527,.T.);
#11833=ADVANCED_FACE('',(#1866),#1188,.T.);
#11834=ADVANCED_FACE('',(#1867),#11528,.T.);
#11835=ADVANCED_FACE('',(#1868),#11529,.T.);
#11836=ADVANCED_FACE('',(#1869),#11530,.T.);
#11837=ADVANCED_FACE('',(#1870),#11531,.T.);
#11838=ADVANCED_FACE('',(#1871),#11532,.T.);
#11839=ADVANCED_FACE('',(#1872),#1189,.T.);
#11840=ADVANCED_FACE('',(#1873),#1190,.F.);
#11841=ADVANCED_FACE('',(#1874),#11533,.T.);
#11842=ADVANCED_FACE('',(#1875),#11534,.T.);
#11843=ADVANCED_FACE('',(#1876),#1191,.T.);
#11844=ADVANCED_FACE('',(#1877),#1192,.F.);
#11845=ADVANCED_FACE('',(#1878,#1348,#1349,#1350,#1351),#11535,.T.);
#11846=ADVANCED_FACE('',(#1879),#1193,.T.);
#11847=ADVANCED_FACE('',(#1880),#11536,.T.);
#11848=ADVANCED_FACE('',(#1881),#11537,.T.);
#11849=ADVANCED_FACE('',(#1882),#11538,.T.);
#11850=ADVANCED_FACE('',(#1883),#11539,.T.);
#11851=ADVANCED_FACE('',(#1884),#11540,.T.);
#11852=ADVANCED_FACE('',(#1885),#11541,.T.);
#11853=ADVANCED_FACE('',(#1886),#1194,.T.);
#11854=ADVANCED_FACE('',(#1887),#1195,.F.);
#11855=ADVANCED_FACE('',(#1888),#362,.F.);
#11856=ADVANCED_FACE('',(#1889),#246,.F.);
#11857=ADVANCED_FACE('',(#1890),#363,.F.);
#11858=ADVANCED_FACE('',(#1891),#364,.F.);
#11859=ADVANCED_FACE('',(#1892),#247,.F.);
#11860=ADVANCED_FACE('',(#1893),#365,.F.);
#11861=ADVANCED_FACE('',(#1894),#366,.F.);
#11862=ADVANCED_FACE('',(#1895),#248,.F.);
#11863=ADVANCED_FACE('',(#1896),#367,.F.);
#11864=ADVANCED_FACE('',(#1897),#368,.F.);
#11865=ADVANCED_FACE('',(#1898),#249,.F.);
#11866=ADVANCED_FACE('',(#1899),#369,.F.);
#11867=ADVANCED_FACE('',(#1900),#370,.F.);
#11868=ADVANCED_FACE('',(#1901),#250,.F.);
#11869=ADVANCED_FACE('',(#1902,#1352),#11542,.F.);
#11870=ADVANCED_FACE('',(#1903),#251,.F.);
#11871=ADVANCED_FACE('',(#1904,#1353),#11543,.F.);
#11872=ADVANCED_FACE('',(#1905),#252,.F.);
#11873=ADVANCED_FACE('',(#1906),#371,.F.);
#11874=ADVANCED_FACE('',(#1907),#372,.F.);
#11875=ADVANCED_FACE('',(#1908),#253,.F.);
#11876=ADVANCED_FACE('',(#1909,#1354),#11544,.F.);
#11877=ADVANCED_FACE('',(#1910),#254,.F.);
#11878=ADVANCED_FACE('',(#1911,#1355),#11545,.F.);
#11879=ADVANCED_FACE('',(#1912),#255,.F.);
#11880=ADVANCED_FACE('',(#1913),#373,.F.);
#11881=ADVANCED_FACE('',(#1914),#374,.F.);
#11882=ADVANCED_FACE('',(#1915),#256,.F.);
#11883=ADVANCED_FACE('',(#1916,#1356),#11546,.F.);
#11884=ADVANCED_FACE('',(#1917),#257,.F.);
#11885=ADVANCED_FACE('',(#1918,#1357),#11547,.F.);
#11886=ADVANCED_FACE('',(#1919),#258,.F.);
#11887=ADVANCED_FACE('',(#1920),#375,.F.);
#11888=ADVANCED_FACE('',(#1921),#1196,.T.);
#11889=ADVANCED_FACE('',(#1922),#1197,.T.);
#11890=ADVANCED_FACE('',(#1923),#11548,.T.);
#11891=ADVANCED_FACE('',(#1924),#11549,.T.);
#11892=ADVANCED_FACE('',(#1925),#11550,.T.);
#11893=ADVANCED_FACE('',(#1926),#11551,.T.);
#11894=ADVANCED_FACE('',(#1927),#11552,.T.);
#11895=ADVANCED_FACE('',(#1928),#11553,.T.);
#11896=ADVANCED_FACE('',(#1929),#11554,.T.);
#11897=ADVANCED_FACE('',(#1930),#1198,.T.);
#11898=ADVANCED_FACE('',(#1931),#1199,.T.);
#11899=ADVANCED_FACE('',(#1932),#1200,.T.);
#11900=ADVANCED_FACE('',(#1933),#1201,.T.);
#11901=ADVANCED_FACE('',(#1934),#1202,.F.);
#11902=ADVANCED_FACE('',(#1935),#1203,.F.);
#11903=ADVANCED_FACE('',(#1936),#1204,.F.);
#11904=ADVANCED_FACE('',(#1937),#1205,.F.);
#11905=ADVANCED_FACE('',(#1938),#227,.F.);
#11906=ADVANCED_FACE('',(#1939),#228,.F.);
#11907=ADVANCED_FACE('',(#1940,#1358),#11555,.T.);
#11908=ADVANCED_FACE('',(#1941),#229,.F.);
#11909=ADVANCED_FACE('',(#1942),#259,.F.);
#11910=ADVANCED_FACE('',(#1943),#230,.F.);
#11911=ADVANCED_FACE('',(#1944),#260,.F.);
#11912=ADVANCED_FACE('',(#1945),#261,.T.);
#11913=ADVANCED_FACE('',(#1946,#1359),#11556,.T.);
#11914=ADVANCED_FACE('',(#1947),#262,.T.);
#11915=ADVANCED_FACE('',(#1948),#376,.T.);
#11916=ADVANCED_FACE('',(#1949),#377,.T.);
#11917=ADVANCED_FACE('',(#1950,#1360),#11557,.T.);
#11918=ADVANCED_FACE('',(#1951),#1206,.T.);
#11919=ADVANCED_FACE('',(#1952),#263,.T.);
#11920=ADVANCED_FACE('',(#1953),#264,.T.);
#11921=ADVANCED_FACE('',(#1954),#265,.F.);
#11922=ADVANCED_FACE('',(#1955),#1207,.T.);
#11923=ADVANCED_FACE('',(#1956),#266,.F.);
#11924=ADVANCED_FACE('',(#1957),#378,.T.);
#11925=ADVANCED_FACE('',(#1958),#1208,.F.);
#11926=ADVANCED_FACE('',(#1959),#1209,.F.);
#11927=ADVANCED_FACE('',(#1960),#1210,.F.);
#11928=ADVANCED_FACE('',(#1961),#379,.T.);
#11929=ADVANCED_FACE('',(#1962),#380,.T.);
#11930=ADVANCED_FACE('',(#1963),#1211,.F.);
#11931=ADVANCED_FACE('',(#1964),#1212,.F.);
#11932=ADVANCED_FACE('',(#1965),#1213,.F.);
#11933=ADVANCED_FACE('',(#1966),#381,.T.);
#11934=ADVANCED_FACE('',(#1967),#1214,.F.);
#11935=ADVANCED_FACE('',(#1968),#1215,.F.);
#11936=ADVANCED_FACE('',(#1969),#1216,.F.);
#11937=ADVANCED_FACE('',(#1970),#382,.T.);
#11938=ADVANCED_FACE('',(#1971),#1217,.F.);
#11939=ADVANCED_FACE('',(#1972),#1218,.F.);
#11940=ADVANCED_FACE('',(#1973),#1219,.F.);
#11941=ADVANCED_FACE('',(#1974),#383,.T.);
#11942=ADVANCED_FACE('',(#1975),#1220,.F.);
#11943=ADVANCED_FACE('',(#1976),#1221,.F.);
#11944=ADVANCED_FACE('',(#1977),#1222,.F.);
#11945=ADVANCED_FACE('',(#1978),#384,.T.);
#11946=ADVANCED_FACE('',(#1979),#1223,.F.);
#11947=ADVANCED_FACE('',(#1980),#1224,.F.);
#11948=ADVANCED_FACE('',(#1981),#1225,.F.);
#11949=ADVANCED_FACE('',(#1982),#385,.T.);
#11950=ADVANCED_FACE('',(#1983),#1226,.F.);
#11951=ADVANCED_FACE('',(#1984),#1227,.F.);
#11952=ADVANCED_FACE('',(#1985),#1228,.F.);
#11953=ADVANCED_FACE('',(#1986),#386,.T.);
#11954=ADVANCED_FACE('',(#1987),#1229,.F.);
#11955=ADVANCED_FACE('',(#1988),#1230,.F.);
#11956=ADVANCED_FACE('',(#1989),#1231,.F.);
#11957=ADVANCED_FACE('',(#1990),#387,.T.);
#11958=ADVANCED_FACE('',(#1991),#1232,.F.);
#11959=ADVANCED_FACE('',(#1992),#1233,.F.);
#11960=ADVANCED_FACE('',(#1993),#1234,.F.);
#11961=ADVANCED_FACE('',(#1994),#388,.T.);
#11962=ADVANCED_FACE('',(#1995),#1235,.F.);
#11963=ADVANCED_FACE('',(#1996),#1236,.F.);
#11964=ADVANCED_FACE('',(#1997),#1237,.F.);
#11965=ADVANCED_FACE('',(#1998),#389,.T.);
#11966=ADVANCED_FACE('',(#1999),#1238,.F.);
#11967=ADVANCED_FACE('',(#2000),#1239,.F.);
#11968=ADVANCED_FACE('',(#2001),#1240,.F.);
#11969=ADVANCED_FACE('',(#2002),#390,.T.);
#11970=ADVANCED_FACE('',(#2003),#1241,.F.);
#11971=ADVANCED_FACE('',(#2004),#1242,.F.);
#11972=ADVANCED_FACE('',(#2005),#1243,.F.);
#11973=ADVANCED_FACE('',(#2006),#391,.T.);
#11974=ADVANCED_FACE('',(#2007),#1244,.F.);
#11975=ADVANCED_FACE('',(#2008),#1245,.F.);
#11976=ADVANCED_FACE('',(#2009),#1246,.F.);
#11977=ADVANCED_FACE('',(#2010),#392,.T.);
#11978=ADVANCED_FACE('',(#2011),#1247,.F.);
#11979=ADVANCED_FACE('',(#2012),#1248,.F.);
#11980=ADVANCED_FACE('',(#2013),#1249,.F.);
#11981=ADVANCED_FACE('',(#2014),#393,.T.);
#11982=ADVANCED_FACE('',(#2015),#1250,.F.);
#11983=ADVANCED_FACE('',(#2016),#1251,.F.);
#11984=ADVANCED_FACE('',(#2017),#1252,.F.);
#11985=ADVANCED_FACE('',(#2018),#394,.T.);
#11986=ADVANCED_FACE('',(#2019),#1253,.F.);
#11987=ADVANCED_FACE('',(#2020),#1254,.F.);
#11988=ADVANCED_FACE('',(#2021),#1255,.F.);
#11989=ADVANCED_FACE('',(#2022),#395,.T.);
#11990=ADVANCED_FACE('',(#2023),#1256,.F.);
#11991=ADVANCED_FACE('',(#2024),#1257,.F.);
#11992=ADVANCED_FACE('',(#2025),#1258,.F.);
#11993=ADVANCED_FACE('',(#2026),#396,.T.);
#11994=ADVANCED_FACE('',(#2027),#1259,.F.);
#11995=ADVANCED_FACE('',(#2028),#1260,.F.);
#11996=ADVANCED_FACE('',(#2029),#1261,.F.);
#11997=ADVANCED_FACE('',(#2030),#397,.T.);
#11998=ADVANCED_FACE('',(#2031),#1262,.F.);
#11999=ADVANCED_FACE('',(#2032),#1263,.F.);
#12000=ADVANCED_FACE('',(#2033),#1264,.F.);
#12001=ADVANCED_FACE('',(#2034),#1265,.F.);
#12002=ADVANCED_FACE('',(#2035),#1266,.F.);
#12003=ADVANCED_FACE('',(#2036),#1267,.F.);
#12004=ADVANCED_FACE('',(#2037),#398,.F.);
#12005=ADVANCED_FACE('',(#2038),#399,.T.);
#12006=ADVANCED_FACE('',(#2039,#1361),#11558,.T.);
#12007=ADVANCED_FACE('',(#2040),#400,.F.);
#12008=ADVANCED_FACE('',(#2041,#1362,#1363),#267,.F.);
#12009=ADVANCED_FACE('',(#2042),#401,.F.);
#12010=ADVANCED_FACE('',(#2043,#1364),#11559,.T.);
#12011=ADVANCED_FACE('',(#2044),#402,.F.);
#12012=ADVANCED_FACE('',(#2045),#268,.F.);
#12013=ADVANCED_FACE('',(#2046,#1365),#11560,.T.);
#12014=ADVANCED_FACE('',(#2047),#403,.F.);
#12015=ADVANCED_FACE('',(#2048),#11561,.F.);
#12016=ADVANCED_FACE('',(#2049),#11562,.F.);
#12017=ADVANCED_FACE('',(#2050),#11563,.F.);
#12018=ADVANCED_FACE('',(#2051),#11564,.F.);
#12019=ADVANCED_FACE('',(#2052),#11565,.F.);
#12020=ADVANCED_FACE('',(#2053),#11566,.F.);
#12021=ADVANCED_FACE('',(#2054),#11567,.T.);
#12022=ADVANCED_FACE('',(#2055),#404,.T.);
#12023=ADVANCED_FACE('',(#2056,#1366,#1367),#269,.T.);
#12024=ADVANCED_FACE('',(#2057,#1368),#11568,.T.);
#12025=ADVANCED_FACE('',(#2058),#270,.T.);
#12026=ADVANCED_FACE('',(#2059,#1369),#11569,.T.);
#12027=ADVANCED_FACE('',(#2060),#271,.T.);
#12028=ADVANCED_FACE('',(#2061),#405,.T.);
#12029=ADVANCED_FACE('',(#2062),#1268,.T.);
#12030=ADVANCED_FACE('',(#2063),#272,.T.);
#12031=ADVANCED_FACE('',(#2064),#273,.T.);
#12032=ADVANCED_FACE('',(#2065),#274,.F.);
#12033=ADVANCED_FACE('',(#2066),#1269,.T.);
#12034=ADVANCED_FACE('',(#2067),#275,.F.);
#12035=ADVANCED_FACE('',(#2068),#406,.T.);
#12036=ADVANCED_FACE('',(#2069),#1270,.F.);
#12037=ADVANCED_FACE('',(#2070),#1271,.F.);
#12038=ADVANCED_FACE('',(#2071),#1272,.F.);
#12039=ADVANCED_FACE('',(#2072),#407,.T.);
#12040=ADVANCED_FACE('',(#2073),#408,.T.);
#12041=ADVANCED_FACE('',(#2074),#409,.T.);
#12042=ADVANCED_FACE('',(#2075),#1273,.F.);
#12043=ADVANCED_FACE('',(#2076),#1274,.F.);
#12044=ADVANCED_FACE('',(#2077),#1275,.F.);
#12045=ADVANCED_FACE('',(#2078),#410,.T.);
#12046=ADVANCED_FACE('',(#2079),#1276,.F.);
#12047=ADVANCED_FACE('',(#2080),#1277,.F.);
#12048=ADVANCED_FACE('',(#2081),#1278,.F.);
#12049=ADVANCED_FACE('',(#2082),#411,.T.);
#12050=ADVANCED_FACE('',(#2083),#1279,.F.);
#12051=ADVANCED_FACE('',(#2084),#1280,.F.);
#12052=ADVANCED_FACE('',(#2085),#1281,.F.);
#12053=ADVANCED_FACE('',(#2086),#412,.T.);
#12054=ADVANCED_FACE('',(#2087),#1282,.F.);
#12055=ADVANCED_FACE('',(#2088),#1283,.F.);
#12056=ADVANCED_FACE('',(#2089),#1284,.F.);
#12057=ADVANCED_FACE('',(#2090),#413,.T.);
#12058=ADVANCED_FACE('',(#2091),#1285,.F.);
#12059=ADVANCED_FACE('',(#2092),#1286,.F.);
#12060=ADVANCED_FACE('',(#2093),#1287,.F.);
#12061=ADVANCED_FACE('',(#2094),#414,.T.);
#12062=ADVANCED_FACE('',(#2095),#1288,.F.);
#12063=ADVANCED_FACE('',(#2096),#1289,.F.);
#12064=ADVANCED_FACE('',(#2097),#1290,.F.);
#12065=ADVANCED_FACE('',(#2098),#415,.T.);
#12066=ADVANCED_FACE('',(#2099),#1291,.F.);
#12067=ADVANCED_FACE('',(#2100),#1292,.F.);
#12068=ADVANCED_FACE('',(#2101),#1293,.F.);
#12069=ADVANCED_FACE('',(#2102),#416,.T.);
#12070=ADVANCED_FACE('',(#2103),#1294,.F.);
#12071=ADVANCED_FACE('',(#2104),#1295,.F.);
#12072=ADVANCED_FACE('',(#2105),#1296,.F.);
#12073=ADVANCED_FACE('',(#2106),#417,.T.);
#12074=ADVANCED_FACE('',(#2107),#1297,.F.);
#12075=ADVANCED_FACE('',(#2108),#1298,.F.);
#12076=ADVANCED_FACE('',(#2109),#1299,.F.);
#12077=ADVANCED_FACE('',(#2110),#418,.T.);
#12078=ADVANCED_FACE('',(#2111),#1300,.F.);
#12079=ADVANCED_FACE('',(#2112),#1301,.F.);
#12080=ADVANCED_FACE('',(#2113),#1302,.F.);
#12081=ADVANCED_FACE('',(#2114),#419,.T.);
#12082=ADVANCED_FACE('',(#2115),#1303,.F.);
#12083=ADVANCED_FACE('',(#2116),#1304,.F.);
#12084=ADVANCED_FACE('',(#2117),#1305,.F.);
#12085=ADVANCED_FACE('',(#2118),#420,.T.);
#12086=ADVANCED_FACE('',(#2119),#1306,.F.);
#12087=ADVANCED_FACE('',(#2120),#1307,.F.);
#12088=ADVANCED_FACE('',(#2121),#1308,.F.);
#12089=ADVANCED_FACE('',(#2122),#421,.T.);
#12090=ADVANCED_FACE('',(#2123),#1309,.F.);
#12091=ADVANCED_FACE('',(#2124),#1310,.F.);
#12092=ADVANCED_FACE('',(#2125),#1311,.F.);
#12093=ADVANCED_FACE('',(#2126),#422,.T.);
#12094=ADVANCED_FACE('',(#2127),#1312,.F.);
#12095=ADVANCED_FACE('',(#2128),#1313,.F.);
#12096=ADVANCED_FACE('',(#2129),#1314,.F.);
#12097=ADVANCED_FACE('',(#2130),#423,.T.);
#12098=ADVANCED_FACE('',(#2131),#1315,.F.);
#12099=ADVANCED_FACE('',(#2132),#1316,.F.);
#12100=ADVANCED_FACE('',(#2133),#1317,.F.);
#12101=ADVANCED_FACE('',(#2134),#424,.T.);
#12102=ADVANCED_FACE('',(#2135),#1318,.F.);
#12103=ADVANCED_FACE('',(#2136),#1319,.F.);
#12104=ADVANCED_FACE('',(#2137),#1320,.F.);
#12105=ADVANCED_FACE('',(#2138),#425,.T.);
#12106=ADVANCED_FACE('',(#2139),#1321,.F.);
#12107=ADVANCED_FACE('',(#2140),#1322,.F.);
#12108=ADVANCED_FACE('',(#2141),#1323,.F.);
#12109=ADVANCED_FACE('',(#2142),#426,.T.);
#12110=ADVANCED_FACE('',(#2143),#1324,.F.);
#12111=ADVANCED_FACE('',(#2144),#1325,.F.);
#12112=ADVANCED_FACE('',(#2145),#1326,.F.);
#12113=ADVANCED_FACE('',(#2146),#1327,.F.);
#12114=ADVANCED_FACE('',(#2147),#1328,.F.);
#12115=ADVANCED_FACE('',(#2148),#1329,.F.);
#12116=ADVANCED_FACE('',(#2149),#427,.F.);
#12117=ADVANCED_FACE('',(#2150),#428,.T.);
#12118=ADVANCED_FACE('',(#2151,#1370),#11570,.T.);
#12119=ADVANCED_FACE('',(#2152,#1371),#11571,.T.);
#12120=ADVANCED_FACE('',(#2153),#429,.F.);
#12121=ADVANCED_FACE('',(#2154,#1372,#1373),#276,.F.);
#12122=ADVANCED_FACE('',(#2155),#430,.F.);
#12123=ADVANCED_FACE('',(#2156,#1374),#11572,.T.);
#12124=ADVANCED_FACE('',(#2157,#1375),#11573,.T.);
#12125=ADVANCED_FACE('',(#2158,#1376),#11574,.T.);
#12126=ADVANCED_FACE('',(#2159),#277,.F.);
#12127=ADVANCED_FACE('',(#2160),#278,.F.);
#12128=ADVANCED_FACE('',(#2161,#1377),#11575,.T.);
#12129=ADVANCED_FACE('',(#2162,#1378),#11576,.T.);
#12130=ADVANCED_FACE('',(#2163),#279,.F.);
#12131=ADVANCED_FACE('',(#2164),#280,.F.);
#12132=ADVANCED_FACE('',(#2165,#1379),#176,.T.);
#12133=ADVANCED_FACE('',(#2166),#281,.F.);
#12134=ADVANCED_FACE('',(#2167),#231,.F.);
#12135=ADVANCED_FACE('',(#2168),#282,.T.);
#12136=ADVANCED_FACE('',(#2169),#232,.F.);
#12137=ADVANCED_FACE('',(#2170,#1380),#177,.T.);
#12138=ADVANCED_FACE('',(#2171),#233,.F.);
#12139=ADVANCED_FACE('',(#2172),#234,.F.);
#12140=ADVANCED_FACE('',(#2173,#1381),#178,.T.);
#12141=ADVANCED_FACE('',(#2174),#235,.F.);
#12142=ADVANCED_FACE('',(#2175),#236,.F.);
#12143=ADVANCED_FACE('',(#2176,#1382),#179,.T.);
#12144=ADVANCED_FACE('',(#2177),#237,.F.);
#12145=ADVANCED_FACE('',(#2178),#238,.F.);
#12146=ADVANCED_FACE('',(#2179,#1383),#180,.T.);
#12147=ADVANCED_FACE('',(#2180),#239,.F.);
#12148=ADVANCED_FACE('',(#2181),#240,.F.);
#12149=ADVANCED_FACE('',(#2182,#1384),#181,.T.);
#12150=ADVANCED_FACE('',(#2183),#283,.F.);
#12151=ADVANCED_FACE('',(#2184),#241,.F.);
#12152=ADVANCED_FACE('',(#2185),#284,.T.);
#12153=ADVANCED_FACE('',(#2186),#242,.F.);
#12154=ADVANCED_FACE('',(#2187,#1385),#182,.T.);
#12155=ADVANCED_FACE('',(#2188),#243,.F.);
#12156=ADVANCED_FACE('',(#2189,#1386),#11577,.T.);
#12157=ADVANCED_FACE('',(#2190),#431,.T.);
#12158=ADVANCED_FACE('',(#2191),#285,.T.);
#12159=ADVANCED_FACE('',(#2192),#432,.T.);
#12160=ADVANCED_FACE('',(#2193,#1387),#11578,.T.);
#12161=ADVANCED_FACE('',(#2194),#244,.F.);
#12162=ADVANCED_FACE('',(#2195),#286,.F.);
#12163=ADVANCED_FACE('',(#2196),#433,.F.);
#12164=ADVANCED_FACE('',(#2197,#1388),#11579,.T.);
#12165=ADVANCED_FACE('',(#2198,#1389),#11580,.T.);
#12166=ADVANCED_FACE('',(#2199),#434,.F.);
#12167=ADVANCED_FACE('',(#2200),#287,.F.);
#12168=ADVANCED_FACE('',(#2201,#1390),#11581,.T.);
#12169=ADVANCED_FACE('',(#2202),#288,.T.);
#12170=ADVANCED_FACE('',(#2203,#1391),#11582,.T.);
#12171=ADVANCED_FACE('',(#2204),#11583,.T.);
#12172=ADVANCED_FACE('',(#2205),#11584,.F.);
#12173=ADVANCED_FACE('',(#2206),#11585,.T.);
#12174=ADVANCED_FACE('',(#2207),#11586,.T.);
#12175=ADVANCED_FACE('',(#2208),#11587,.F.);
#12176=ADVANCED_FACE('',(#2209),#289,.F.);
#12177=ADVANCED_FACE('',(#2210),#11588,.T.);
#12178=ADVANCED_FACE('',(#2211,#1392,#1393),#11589,.T.);
#12179=ADVANCED_FACE('',(#2212),#11590,.T.);
#12180=ADVANCED_FACE('',(#2213),#11591,.T.);
#12181=ADVANCED_FACE('',(#2214),#290,.F.);
#12182=ADVANCED_FACE('',(#2215),#291,.F.);
#12183=ADVANCED_FACE('',(#2216),#11592,.T.);
#12184=ADVANCED_FACE('',(#2217),#11593,.T.);
#12185=ADVANCED_FACE('',(#2218),#11594,.T.);
#12186=ADVANCED_FACE('',(#2219),#11595,.T.);
#12187=ADVANCED_FACE('',(#2220,#1394,#1395),#11596,.F.);
#12188=ADVANCED_FACE('',(#2221),#292,.T.);
#12189=ADVANCED_FACE('',(#2222),#293,.T.);
#12190=ADVANCED_FACE('',(#2223),#294,.T.);
#12191=ADVANCED_FACE('',(#2224),#295,.T.);
#12192=ADVANCED_FACE('',(#2225),#296,.T.);
#12193=ADVANCED_FACE('',(#2226),#297,.T.);
#12194=ADVANCED_FACE('',(#2227),#298,.T.);
#12195=ADVANCED_FACE('',(#2228),#299,.T.);
#12196=ADVANCED_FACE('',(#2229),#300,.T.);
#12197=ADVANCED_FACE('',(#2230),#301,.T.);
#12198=ADVANCED_FACE('',(#2231),#302,.T.);
#12199=ADVANCED_FACE('',(#2232),#303,.T.);
#12200=ADVANCED_FACE('',(#2233),#304,.T.);
#12201=ADVANCED_FACE('',(#2234),#11597,.T.);
#12202=ADVANCED_FACE('',(#2235),#1330,.F.);
#12203=ADVANCED_FACE('',(#2236),#11598,.F.);
#12204=ADVANCED_FACE('',(#2237),#305,.T.);
#12205=ADVANCED_FACE('',(#2238),#1331,.F.);
#12206=ADVANCED_FACE('',(#2239),#11599,.F.);
#12207=ADVANCED_FACE('',(#2240),#11600,.F.);
#12208=ADVANCED_FACE('',(#2241),#11601,.F.);
#12209=ADVANCED_FACE('',(#2242),#11602,.F.);
#12210=ADVANCED_FACE('',(#2243),#11603,.F.);
#12211=ADVANCED_FACE('',(#2244),#11604,.F.);
#12212=ADVANCED_FACE('',(#2245),#11605,.F.);
#12213=ADVANCED_FACE('',(#2246,#1396),#11606,.T.);
#12214=ADVANCED_FACE('',(#2247),#435,.T.);
#12215=ADVANCED_FACE('',(#2248),#306,.T.);
#12216=ADVANCED_FACE('',(#2249),#436,.T.);
#12217=ADVANCED_FACE('',(#2250),#11607,.T.);
#12218=ADVANCED_FACE('',(#2251),#307,.T.);
#12219=ADVANCED_FACE('',(#2252),#308,.T.);
#12220=ADVANCED_FACE('',(#2253),#309,.T.);
#12221=ADVANCED_FACE('',(#2254),#310,.T.);
#12222=ADVANCED_FACE('',(#2255),#311,.T.);
#12223=ADVANCED_FACE('',(#2256),#312,.T.);
#12224=ADVANCED_FACE('',(#2257),#313,.T.);
#12225=ADVANCED_FACE('',(#2258),#314,.T.);
#12226=ADVANCED_FACE('',(#2259),#315,.T.);
#12227=ADVANCED_FACE('',(#2260),#316,.T.);
#12228=ADVANCED_FACE('',(#2261),#317,.T.);
#12229=ADVANCED_FACE('',(#2262),#318,.T.);
#12230=ADVANCED_FACE('',(#2263),#319,.T.);
#12231=ADVANCED_FACE('',(#2264),#320,.T.);
#12232=ADVANCED_FACE('',(#2265),#321,.T.);
#12233=ADVANCED_FACE('',(#2266),#322,.T.);
#12234=ADVANCED_FACE('',(#2267),#323,.T.);
#12235=ADVANCED_FACE('',(#2268),#324,.T.);
#12236=ADVANCED_FACE('',(#2269),#325,.T.);
#12237=ADVANCED_FACE('',(#2270),#326,.T.);
#12238=ADVANCED_FACE('',(#2271),#327,.T.);
#12239=ADVANCED_FACE('',(#2272),#328,.T.);
#12240=ADVANCED_FACE('',(#2273),#329,.T.);
#12241=ADVANCED_FACE('',(#2274),#330,.T.);
#12242=ADVANCED_FACE('',(#2275),#331,.T.);
#12243=ADVANCED_FACE('',(#2276),#332,.T.);
#12244=ADVANCED_FACE('',(#2277),#333,.T.);
#12245=ADVANCED_FACE('',(#2278),#334,.T.);
#12246=ADVANCED_FACE('',(#2279),#335,.T.);
#12247=ADVANCED_FACE('',(#2280),#336,.T.);
#12248=ADVANCED_FACE('',(#2281),#337,.T.);
#12249=ADVANCED_FACE('',(#2282),#338,.T.);
#12250=ADVANCED_FACE('',(#2283),#339,.T.);
#12251=ADVANCED_FACE('',(#2284),#340,.T.);
#12252=ADVANCED_FACE('',(#2285),#341,.T.);
#12253=ADVANCED_FACE('',(#2286),#342,.T.);
#12254=ADVANCED_FACE('',(#2287),#343,.T.);
#12255=ADVANCED_FACE('',(#2288),#344,.T.);
#12256=ADVANCED_FACE('',(#2289),#345,.T.);
#12257=ADVANCED_FACE('',(#2290),#346,.T.);
#12258=ADVANCED_FACE('',(#2291),#347,.T.);
#12259=ADVANCED_FACE('',(#2292),#348,.T.);
#12260=ADVANCED_FACE('',(#2293),#349,.T.);
#12261=ADVANCED_FACE('',(#2294),#350,.T.);
#12262=ADVANCED_FACE('',(#2295),#351,.T.);
#12263=ADVANCED_FACE('',(#2296),#352,.T.);
#12264=ADVANCED_FACE('',(#2297),#353,.T.);
#12265=ADVANCED_FACE('',(#2298),#354,.T.);
#12266=ADVANCED_FACE('',(#2299),#1332,.F.);
#12267=ADVANCED_FACE('',(#2300),#11608,.T.);
#12268=ADVANCED_FACE('',(#2301),#355,.T.);
#12269=ADVANCED_FACE('',(#2302),#1333,.F.);
#12270=ADVANCED_FACE('',(#2303),#437,.F.);
#12271=ADVANCED_FACE('',(#2304),#11609,.F.);
#12272=ADVANCED_FACE('',(#2305),#11610,.F.);
#12273=ADVANCED_FACE('',(#2306),#11611,.F.);
#12274=ADVANCED_FACE('',(#2307),#11612,.F.);
#12275=ADVANCED_FACE('',(#2308),#11613,.F.);
#12276=ADVANCED_FACE('',(#2309),#11614,.F.);
#12277=ADVANCED_FACE('',(#2310,#1397),#11615,.F.);
#12278=ADVANCED_FACE('',(#2311),#11616,.F.);
#12279=ADVANCED_FACE('',(#2312),#11617,.F.);
#12280=ADVANCED_FACE('',(#2313),#11618,.F.);
#12281=ADVANCED_FACE('',(#2314),#11619,.F.);
#12282=ADVANCED_FACE('',(#2315),#11620,.F.);
#12283=ADVANCED_FACE('',(#2316),#11621,.F.);
#12284=ADVANCED_FACE('',(#2317),#11622,.F.);
#12285=ADVANCED_FACE('',(#2318),#11623,.F.);
#12286=ADVANCED_FACE('',(#2319),#11624,.F.);
#12287=ADVANCED_FACE('',(#2320),#11625,.F.);
#12288=ADVANCED_FACE('',(#2321),#11626,.F.);
#12289=ADVANCED_FACE('',(#2322),#11627,.F.);
#12290=ADVANCED_FACE('',(#2323),#11628,.F.);
#12291=ADVANCED_FACE('',(#2324),#11629,.F.);
#12292=ADVANCED_FACE('',(#2325),#11630,.F.);
#12293=ADVANCED_FACE('',(#2326),#11631,.F.);
#12294=ADVANCED_FACE('',(#2327),#11632,.F.);
#12295=ADVANCED_FACE('',(#2328),#11633,.F.);
#12296=ADVANCED_FACE('',(#2329),#11634,.F.);
#12297=ADVANCED_FACE('',(#2330),#11635,.F.);
#12298=ADVANCED_FACE('',(#2331),#11636,.F.);
#12299=ADVANCED_FACE('',(#2332),#11637,.F.);
#12300=ADVANCED_FACE('',(#2333),#11638,.F.);
#12301=ADVANCED_FACE('',(#2334),#11639,.F.);
#12302=ADVANCED_FACE('',(#2335),#11640,.F.);
#12303=ADVANCED_FACE('',(#2336),#11641,.F.);
#12304=ADVANCED_FACE('',(#2337),#11642,.F.);
#12305=ADVANCED_FACE('',(#2338),#11643,.F.);
#12306=ADVANCED_FACE('',(#2339),#11644,.F.);
#12307=ADVANCED_FACE('',(#2340),#11645,.F.);
#12308=ADVANCED_FACE('',(#2341),#11646,.F.);
#12309=ADVANCED_FACE('',(#2342),#11647,.F.);
#12310=ADVANCED_FACE('',(#2343),#11648,.F.);
#12311=ADVANCED_FACE('',(#2344),#11649,.F.);
#12312=ADVANCED_FACE('',(#2345),#11650,.F.);
#12313=ADVANCED_FACE('',(#2346),#11651,.F.);
#12314=ADVANCED_FACE('',(#2347),#11652,.F.);
#12315=ADVANCED_FACE('',(#2348),#11653,.F.);
#12316=ADVANCED_FACE('',(#2349),#11654,.F.);
#12317=ADVANCED_FACE('',(#2350),#11655,.F.);
#12318=ADVANCED_FACE('',(#2351),#11656,.F.);
#12319=ADVANCED_FACE('',(#2352),#11657,.F.);
#12320=ADVANCED_FACE('',(#2353),#11658,.F.);
#12321=ADVANCED_FACE('',(#2354),#11659,.F.);
#12322=ADVANCED_FACE('',(#2355),#11660,.F.);
#12323=ADVANCED_FACE('',(#2356),#11661,.F.);
#12324=ADVANCED_FACE('',(#2357),#11662,.F.);
#12325=ADVANCED_FACE('',(#2358),#11663,.F.);
#12326=ADVANCED_FACE('',(#2359),#11664,.F.);
#12327=ADVANCED_FACE('',(#2360),#11665,.F.);
#12328=ADVANCED_FACE('',(#2361),#11666,.F.);
#12329=ADVANCED_FACE('',(#2362),#11667,.F.);
#12330=ADVANCED_FACE('',(#2363),#11668,.F.);
#12331=ADVANCED_FACE('',(#2364),#11669,.F.);
#12332=ADVANCED_FACE('',(#2365),#11670,.F.);
#12333=ADVANCED_FACE('',(#2366),#11671,.F.);
#12334=ADVANCED_FACE('',(#2367),#11672,.F.);
#12335=ADVANCED_FACE('',(#2368),#11673,.F.);
#12336=ADVANCED_FACE('',(#2369),#11674,.F.);
#12337=ADVANCED_FACE('',(#2370),#11675,.F.);
#12338=ADVANCED_FACE('',(#2371),#11676,.F.);
#12339=ADVANCED_FACE('',(#2372),#11677,.F.);
#12340=ADVANCED_FACE('',(#2373),#11678,.F.);
#12341=ADVANCED_FACE('',(#2374),#11679,.F.);
#12342=ADVANCED_FACE('',(#2375),#11680,.F.);
#12343=ADVANCED_FACE('',(#2376),#11681,.F.);
#12344=ADVANCED_FACE('',(#2377),#11682,.F.);
#12345=ADVANCED_FACE('',(#2378),#11683,.F.);
#12346=ADVANCED_FACE('',(#2379),#11684,.F.);
#12347=ADVANCED_FACE('',(#2380),#11685,.F.);
#12348=ADVANCED_FACE('',(#2381),#11686,.F.);
#12349=ADVANCED_FACE('',(#2382),#11687,.F.);
#12350=ADVANCED_FACE('',(#2383),#11688,.F.);
#12351=ADVANCED_FACE('',(#2384),#11689,.F.);
#12352=ADVANCED_FACE('',(#2385),#11690,.F.);
#12353=ADVANCED_FACE('',(#2386),#11691,.F.);
#12354=ADVANCED_FACE('',(#2387),#11692,.F.);
#12355=ADVANCED_FACE('',(#2388),#11693,.F.);
#12356=ADVANCED_FACE('',(#2389),#11694,.F.);
#12357=ADVANCED_FACE('',(#2390),#11695,.F.);
#12358=ADVANCED_FACE('',(#2391),#11696,.F.);
#12359=ADVANCED_FACE('',(#2392),#11697,.F.);
#12360=ADVANCED_FACE('',(#2393),#11698,.F.);
#12361=ADVANCED_FACE('',(#2394),#11699,.F.);
#12362=ADVANCED_FACE('',(#2395),#11700,.F.);
#12363=ADVANCED_FACE('',(#2396),#11701,.F.);
#12364=ADVANCED_FACE('',(#2397),#11702,.F.);
#12365=ADVANCED_FACE('',(#2398),#11703,.F.);
#12366=ADVANCED_FACE('',(#2399),#11704,.F.);
#12367=ADVANCED_FACE('',(#2400),#11705,.F.);
#12368=ADVANCED_FACE('',(#2401),#11706,.F.);
#12369=ADVANCED_FACE('',(#2402),#11707,.F.);
#12370=ADVANCED_FACE('',(#2403),#11708,.F.);
#12371=ADVANCED_FACE('',(#2404),#11709,.F.);
#12372=ADVANCED_FACE('',(#2405),#11710,.F.);
#12373=ADVANCED_FACE('',(#2406),#11711,.F.);
#12374=ADVANCED_FACE('',(#2407),#11712,.F.);
#12375=ADVANCED_FACE('',(#2408),#11713,.F.);
#12376=ADVANCED_FACE('',(#2409),#11714,.F.);
#12377=ADVANCED_FACE('',(#2410),#11715,.F.);
#12378=ADVANCED_FACE('',(#2411),#11716,.F.);
#12379=ADVANCED_FACE('',(#2412),#11717,.F.);
#12380=ADVANCED_FACE('',(#2413),#11718,.F.);
#12381=ADVANCED_FACE('',(#2414),#11719,.F.);
#12382=ADVANCED_FACE('',(#2415),#11720,.F.);
#12383=ADVANCED_FACE('',(#2416),#11721,.F.);
#12384=ADVANCED_FACE('',(#2417),#11722,.F.);
#12385=ADVANCED_FACE('',(#2418),#11723,.F.);
#12386=ADVANCED_FACE('',(#2419),#11724,.F.);
#12387=ADVANCED_FACE('',(#2420),#11725,.F.);
#12388=ADVANCED_FACE('',(#2421),#11726,.F.);
#12389=ADVANCED_FACE('',(#2422),#11727,.F.);
#12390=ADVANCED_FACE('',(#2423),#11728,.F.);
#12391=ADVANCED_FACE('',(#2424),#11729,.F.);
#12392=ADVANCED_FACE('',(#2425),#11730,.F.);
#12393=ADVANCED_FACE('',(#2426),#11731,.F.);
#12394=ADVANCED_FACE('',(#2427),#11732,.F.);
#12395=ADVANCED_FACE('',(#2428),#11733,.F.);
#12396=ADVANCED_FACE('',(#2429),#11734,.F.);
#12397=ADVANCED_FACE('',(#2430),#11735,.F.);
#12398=ADVANCED_FACE('',(#2431),#11736,.F.);
#12399=ADVANCED_FACE('',(#2432),#11737,.F.);
#12400=ADVANCED_FACE('',(#2433),#11738,.F.);
#12401=ADVANCED_FACE('',(#2434),#11739,.F.);
#12402=ADVANCED_FACE('',(#2435),#11740,.F.);
#12403=ADVANCED_FACE('',(#2436),#11741,.F.);
#12404=ADVANCED_FACE('',(#2437),#11742,.F.);
#12405=ADVANCED_FACE('',(#2438),#11743,.F.);
#12406=ADVANCED_FACE('',(#2439),#11744,.F.);
#12407=ADVANCED_FACE('',(#2440),#11745,.F.);
#12408=ADVANCED_FACE('',(#2441),#11746,.F.);
#12409=ADVANCED_FACE('',(#2442),#11747,.F.);
#12410=ADVANCED_FACE('',(#2443),#11748,.F.);
#12411=ADVANCED_FACE('',(#2444),#11749,.F.);
#12412=ADVANCED_FACE('',(#2445),#11750,.F.);
#12413=ADVANCED_FACE('',(#2446),#11751,.F.);
#12414=ADVANCED_FACE('',(#2447),#11752,.F.);
#12415=ADVANCED_FACE('',(#2448),#11753,.F.);
#12416=ADVANCED_FACE('',(#2449),#11754,.F.);
#12417=ADVANCED_FACE('',(#2450),#11755,.F.);
#12418=ADVANCED_FACE('',(#2451),#11756,.F.);
#12419=ADVANCED_FACE('',(#2452),#11757,.F.);
#12420=ADVANCED_FACE('',(#2453),#11758,.F.);
#12421=ADVANCED_FACE('',(#2454),#11759,.F.);
#12422=ADVANCED_FACE('',(#2455),#245,.F.);
#12423=ADVANCED_FACE('',(#2456),#356,.T.);
#12424=ADVANCED_FACE('',(#2457,#1398),#11760,.T.);
#12425=ADVANCED_FACE('',(#2458),#11761,.T.);
#12426=ADVANCED_FACE('',(#2459),#438,.T.);
#12427=ADVANCED_FACE('',(#2460),#357,.T.);
#12428=ADVANCED_FACE('',(#2461,#1399),#11762,.F.);
#12429=ADVANCED_FACE('',(#2462),#439,.T.);
#12430=ADVANCED_FACE('',(#2463),#358,.T.);
#12431=ADVANCED_FACE('',(#2464),#440,.T.);
#12432=ADVANCED_FACE('',(#2465,#1400),#11763,.T.);
#12433=ADVANCED_FACE('',(#2466),#441,.T.);
#12434=ADVANCED_FACE('',(#2467,#1401),#11764,.T.);
#12435=ADVANCED_FACE('',(#2468),#359,.T.);
#12436=ADVANCED_FACE('',(#2469),#442,.F.);
#12437=ADVANCED_FACE('',(#2470),#360,.F.);
#12438=ADVANCED_FACE('',(#2471,#1402),#11765,.T.);
#12439=ADVANCED_FACE('',(#2472),#443,.F.);
#12440=ADVANCED_FACE('',(#2473),#444,.T.);
#12441=ADVANCED_FACE('',(#2474),#11766,.T.);
#12442=ADVANCED_FACE('',(#2475),#11767,.T.);
#12443=ADVANCED_FACE('',(#2476),#11768,.T.);
#12444=ADVANCED_FACE('',(#2477),#11769,.T.);
#12445=ADVANCED_FACE('',(#2478),#11770,.T.);
#12446=ADVANCED_FACE('',(#2479),#11771,.T.);
#12447=ADVANCED_FACE('',(#2480),#1334,.T.);
#12448=ADVANCED_FACE('',(#2481),#11772,.T.);
#12449=ADVANCED_FACE('',(#2482),#1335,.T.);
#12450=ADVANCED_FACE('',(#2483),#1336,.T.);
#12451=ADVANCED_FACE('',(#2484),#11773,.T.);
#12452=ADVANCED_FACE('',(#2485),#11774,.T.);
#12453=ADVANCED_FACE('',(#2486),#1337,.T.);
#12454=ADVANCED_FACE('',(#2487),#1338,.T.);
#12455=ADVANCED_FACE('',(#2488),#11775,.T.);
#12456=ADVANCED_FACE('',(#2489),#11776,.T.);
#12457=ADVANCED_FACE('',(#2490),#1339,.T.);
#12458=ADVANCED_FACE('',(#2491),#11777,.T.);
#12459=ADVANCED_FACE('',(#2492),#11778,.T.);
#12460=ADVANCED_FACE('',(#2493),#11779,.T.);
#12461=ADVANCED_FACE('',(#2494),#11780,.T.);
#12462=ADVANCED_FACE('',(#2495),#445,.T.);
#12463=ADVANCED_FACE('',(#2496),#446,.T.);
#12464=ADVANCED_FACE('',(#2497),#447,.T.);
#12465=ADVANCED_FACE('',(#2498),#448,.T.);
#12466=ADVANCED_FACE('',(#2499),#449,.T.);
#12467=ADVANCED_FACE('',(#2500),#450,.T.);
#12468=ADVANCED_FACE('',(#2501),#451,.T.);
#12469=ADVANCED_FACE('',(#2502),#452,.T.);
#12470=ADVANCED_FACE('',(#2503,#1403),#11781,.T.);
#12471=ADVANCED_FACE('',(#2504),#453,.F.);
#12472=ADVANCED_FACE('',(#2505),#454,.F.);
#12473=ADVANCED_FACE('',(#2506),#455,.F.);
#12474=ADVANCED_FACE('',(#2507),#361,.F.);
#12475=ADVANCED_FACE('',(#2508),#456,.F.);
#12476=ADVANCED_FACE('',(#2509,#1404),#11782,.F.);
#12477=ADVANCED_FACE('',(#2510),#11783,.T.);
#12478=ADVANCED_FACE('',(#2511),#11784,.T.);
#12479=ADVANCED_FACE('',(#2512),#11785,.T.);
#12480=CLOSED_SHELL('',(#11786,#11787,#11788,#11789,#11790,#11791,#11792,
#11793,#11794,#11795,#11796,#11797,#11798,#11799,#11800,#11801,#11802,#11803,
#11804,#11805,#11806,#11807,#11808,#11809,#11810,#11811,#11812,#11813,#11814,
#11815,#11816,#11817,#11818,#11819,#11820,#11821,#11822,#11823,#11824,#11825,
#11826,#11827,#11828,#11829,#11830,#11831,#11832,#11833,#11834,#11835,#11836,
#11837,#11838,#11839,#11840,#11841,#11842,#11843,#11844,#11845,#11846,#11847,
#11848,#11849,#11850,#11851,#11852,#11853,#11854,#11855,#11856,#11857,#11858,
#11859,#11860,#11861,#11862,#11863,#11864,#11865,#11866,#11867,#11868,#11869,
#11870,#11871,#11872,#11873,#11874,#11875,#11876,#11877,#11878,#11879,#11880,
#11881,#11882,#11883,#11884,#11885,#11886,#11887,#11888,#11889,#11890,#11891,
#11892,#11893,#11894,#11895,#11896,#11897,#11898,#11899,#11900,#11901,#11902,
#11903,#11904,#11905,#11906,#11907,#11908,#11909,#11910,#11911,#11912,#11913,
#11914));
#12481=CLOSED_SHELL('',(#11915,#11916,#11917,#11918,#11919,#11920,#11921,
#11922,#11923,#11924,#11925,#11926,#11927,#11928,#11929,#11930,#11931,#11932,
#11933,#11934,#11935,#11936,#11937,#11938,#11939,#11940,#11941,#11942,#11943,
#11944,#11945,#11946,#11947,#11948,#11949,#11950,#11951,#11952,#11953,#11954,
#11955,#11956,#11957,#11958,#11959,#11960,#11961,#11962,#11963,#11964,#11965,
#11966,#11967,#11968,#11969,#11970,#11971,#11972,#11973,#11974,#11975,#11976,
#11977,#11978,#11979,#11980,#11981,#11982,#11983,#11984,#11985,#11986,#11987,
#11988,#11989,#11990,#11991,#11992,#11993,#11994,#11995,#11996,#11997,#11998,
#11999,#12000,#12001,#12002,#12003,#12004,#12005,#12006,#12007,#12008,#12009,
#12010));
#12482=CLOSED_SHELL('',(#12011,#12012,#12013,#12014,#12015,#12016,#12017,
#12018,#12019,#12020,#12021,#12022,#12023,#12024,#12025,#12026,#12027,#12028));
#12483=CLOSED_SHELL('',(#12029,#12030,#12031,#12032,#12033,#12034,#12035,
#12036,#12037,#12038,#12039,#12040,#12041,#12042,#12043,#12044,#12045,#12046,
#12047,#12048,#12049,#12050,#12051,#12052,#12053,#12054,#12055,#12056,#12057,
#12058,#12059,#12060,#12061,#12062,#12063,#12064,#12065,#12066,#12067,#12068,
#12069,#12070,#12071,#12072,#12073,#12074,#12075,#12076,#12077,#12078,#12079,
#12080,#12081,#12082,#12083,#12084,#12085,#12086,#12087,#12088,#12089,#12090,
#12091,#12092,#12093,#12094,#12095,#12096,#12097,#12098,#12099,#12100,#12101,
#12102,#12103,#12104,#12105,#12106,#12107,#12108,#12109,#12110,#12111,#12112,
#12113,#12114,#12115,#12116,#12117,#12118,#12119,#12120,#12121,#12122,#12123));
#12484=CLOSED_SHELL('',(#12124,#12125,#12126,#12127,#12128,#12129,#12130,
#12131,#12132,#12133,#12134,#12135,#12136,#12137,#12138,#12139,#12140,#12141,
#12142,#12143,#12144,#12145,#12146,#12147,#12148,#12149,#12150,#12151,#12152,
#12153,#12154,#12155,#12156,#12157,#12158,#12159,#12160,#12161,#12162,#12163,
#12164,#12165,#12166));
#12485=CLOSED_SHELL('',(#12167,#12168,#12169,#12170));
#12486=CLOSED_SHELL('',(#12171,#12172,#12173,#12174,#12175,#12176,#12177,
#12178,#12179,#12180,#12181,#12182,#12183,#12184,#12185,#12186,#12187,#12188));
#12487=CLOSED_SHELL('',(#12189,#12190,#12191,#12192,#12193,#12194,#12195,
#12196,#12197,#12198,#12199,#12200,#12201,#12202,#12203,#12204,#12205,#12206,
#12207,#12208,#12209,#12210,#12211,#12212,#12213,#12214,#12215,#12216,#12217));
#12488=CLOSED_SHELL('',(#12218,#12219,#12220,#12221,#12222,#12223,#12224,
#12225,#12226,#12227,#12228,#12229,#12230,#12231,#12232,#12233,#12234,#12235,
#12236,#12237,#12238,#12239,#12240,#12241,#12242,#12243,#12244,#12245,#12246,
#12247,#12248,#12249,#12250,#12251,#12252,#12253,#12254,#12255,#12256,#12257,
#12258,#12259,#12260,#12261,#12262,#12263,#12264,#12265,#12266,#12267,#12268,
#12269,#12270,#12271,#12272,#12273,#12274,#12275,#12276,#12277,#12278,#12279,
#12280,#12281,#12282,#12283,#12284,#12285,#12286,#12287,#12288,#12289,#12290,
#12291,#12292,#12293,#12294,#12295,#12296,#12297,#12298,#12299,#12300,#12301,
#12302,#12303,#12304,#12305,#12306,#12307,#12308,#12309,#12310,#12311,#12312,
#12313,#12314,#12315,#12316,#12317,#12318,#12319,#12320,#12321,#12322,#12323,
#12324,#12325,#12326,#12327,#12328,#12329,#12330,#12331,#12332,#12333,#12334,
#12335,#12336,#12337,#12338,#12339,#12340,#12341,#12342,#12343,#12344,#12345,
#12346,#12347,#12348,#12349,#12350,#12351,#12352,#12353,#12354,#12355,#12356,
#12357,#12358,#12359,#12360,#12361,#12362,#12363,#12364,#12365,#12366,#12367,
#12368,#12369,#12370,#12371,#12372,#12373,#12374,#12375,#12376,#12377,#12378,
#12379,#12380,#12381,#12382,#12383,#12384,#12385,#12386,#12387,#12388,#12389,
#12390,#12391,#12392,#12393,#12394,#12395,#12396,#12397,#12398,#12399,#12400,
#12401,#12402,#12403,#12404,#12405,#12406,#12407,#12408,#12409,#12410,#12411,
#12412,#12413,#12414,#12415,#12416,#12417,#12418,#12419,#12420,#12421,#12422,
#12423,#12424,#12425,#12426,#12427,#12428,#12429,#12430,#12431,#12432));
#12489=CLOSED_SHELL('',(#12433,#12434,#12435,#12436,#12437,#12438,#12439,
#12440));
#12490=CLOSED_SHELL('',(#12441,#12442,#12443,#12444,#12445,#12446,#12447,
#12448,#12449,#12450,#12451,#12452,#12453,#12454,#12455,#12456,#12457,#12458,
#12459,#12460,#12461,#12462,#12463,#12464,#12465,#12466,#12467,#12468,#12469,
#12470,#12471,#12472,#12473,#12474,#12475,#12476,#12477,#12478,#12479));
#12491=DERIVED_UNIT_ELEMENT(#12513,1.);
#12492=DERIVED_UNIT_ELEMENT(#31640,-3.);
#12493=DERIVED_UNIT_ELEMENT(#12513,1.);
#12494=DERIVED_UNIT_ELEMENT(#31640,-3.);
#12495=DERIVED_UNIT_ELEMENT(#12513,1.);
#12496=DERIVED_UNIT_ELEMENT(#31640,-3.);
#12497=DERIVED_UNIT_ELEMENT(#12513,1.);
#12498=DERIVED_UNIT_ELEMENT(#31640,-3.);
#12499=DERIVED_UNIT_ELEMENT(#12513,1.);
#12500=DERIVED_UNIT_ELEMENT(#31640,-3.);
#12501=DERIVED_UNIT_ELEMENT(#12513,1.);
#12502=DERIVED_UNIT_ELEMENT(#31640,-3.);
#12503=DERIVED_UNIT_ELEMENT(#12513,1.);
#12504=DERIVED_UNIT_ELEMENT(#31640,-3.);
#12505=DERIVED_UNIT_ELEMENT(#12513,1.);
#12506=DERIVED_UNIT_ELEMENT(#31640,-3.);
#12507=DERIVED_UNIT_ELEMENT(#12513,1.);
#12508=DERIVED_UNIT_ELEMENT(#31640,-3.);
#12509=DERIVED_UNIT_ELEMENT(#12513,1.);
#12510=DERIVED_UNIT_ELEMENT(#31640,-3.);
#12511=DERIVED_UNIT_ELEMENT(#12513,1.);
#12512=DERIVED_UNIT_ELEMENT(#31640,-3.);
#12513=(
MASS_UNIT()
NAMED_UNIT(*)
SI_UNIT(.KILO.,.GRAM.)
);
#12514=DERIVED_UNIT((#12491,#12492));
#12515=DERIVED_UNIT((#12493,#12494));
#12516=DERIVED_UNIT((#12495,#12496));
#12517=DERIVED_UNIT((#12497,#12498));
#12518=DERIVED_UNIT((#12499,#12500));
#12519=DERIVED_UNIT((#12501,#12502));
#12520=DERIVED_UNIT((#12503,#12504));
#12521=DERIVED_UNIT((#12505,#12506));
#12522=DERIVED_UNIT((#12507,#12508));
#12523=DERIVED_UNIT((#12509,#12510));
#12524=DERIVED_UNIT((#12511,#12512));
#12525=MEASURE_REPRESENTATION_ITEM('density measure',
POSITIVE_RATIO_MEASURE(2700.),#12514);
#12526=MEASURE_REPRESENTATION_ITEM('density measure',
POSITIVE_RATIO_MEASURE(7850.),#12515);
#12527=MEASURE_REPRESENTATION_ITEM('density measure',
POSITIVE_RATIO_MEASURE(7850.),#12516);
#12528=MEASURE_REPRESENTATION_ITEM('density measure',
POSITIVE_RATIO_MEASURE(7850.),#12517);
#12529=MEASURE_REPRESENTATION_ITEM('density measure',
POSITIVE_RATIO_MEASURE(7850.),#12518);
#12530=MEASURE_REPRESENTATION_ITEM('density measure',
POSITIVE_RATIO_MEASURE(7850.),#12519);
#12531=MEASURE_REPRESENTATION_ITEM('density measure',
POSITIVE_RATIO_MEASURE(7850.),#12520);
#12532=MEASURE_REPRESENTATION_ITEM('density measure',
POSITIVE_RATIO_MEASURE(7850.),#12521);
#12533=MEASURE_REPRESENTATION_ITEM('density measure',
POSITIVE_RATIO_MEASURE(7850.),#12522);
#12534=MEASURE_REPRESENTATION_ITEM('density measure',
POSITIVE_RATIO_MEASURE(7850.),#12523);
#12535=MEASURE_REPRESENTATION_ITEM('density measure',
POSITIVE_RATIO_MEASURE(7850.),#12524);
#12536=PROPERTY_DEFINITION_REPRESENTATION(#12591,#12558);
#12537=PROPERTY_DEFINITION_REPRESENTATION(#12592,#12559);
#12538=PROPERTY_DEFINITION_REPRESENTATION(#12593,#12560);
#12539=PROPERTY_DEFINITION_REPRESENTATION(#12594,#12561);
#12540=PROPERTY_DEFINITION_REPRESENTATION(#12595,#12562);
#12541=PROPERTY_DEFINITION_REPRESENTATION(#12596,#12563);
#12542=PROPERTY_DEFINITION_REPRESENTATION(#12597,#12564);
#12543=PROPERTY_DEFINITION_REPRESENTATION(#12598,#12565);
#12544=PROPERTY_DEFINITION_REPRESENTATION(#12599,#12566);
#12545=PROPERTY_DEFINITION_REPRESENTATION(#12600,#12567);
#12546=PROPERTY_DEFINITION_REPRESENTATION(#12601,#12568);
#12547=PROPERTY_DEFINITION_REPRESENTATION(#12602,#12569);
#12548=PROPERTY_DEFINITION_REPRESENTATION(#12603,#12570);
#12549=PROPERTY_DEFINITION_REPRESENTATION(#12604,#12571);
#12550=PROPERTY_DEFINITION_REPRESENTATION(#12605,#12572);
#12551=PROPERTY_DEFINITION_REPRESENTATION(#12606,#12573);
#12552=PROPERTY_DEFINITION_REPRESENTATION(#12607,#12574);
#12553=PROPERTY_DEFINITION_REPRESENTATION(#12608,#12575);
#12554=PROPERTY_DEFINITION_REPRESENTATION(#12609,#12576);
#12555=PROPERTY_DEFINITION_REPRESENTATION(#12610,#12577);
#12556=PROPERTY_DEFINITION_REPRESENTATION(#12611,#12578);
#12557=PROPERTY_DEFINITION_REPRESENTATION(#12612,#12579);
#12558=REPRESENTATION('material name',(#12580),#31627);
#12559=REPRESENTATION('density',(#12525),#31627);
#12560=REPRESENTATION('material name',(#12581),#31628);
#12561=REPRESENTATION('density',(#12526),#31628);
#12562=REPRESENTATION('material name',(#12582),#31629);
#12563=REPRESENTATION('density',(#12527),#31629);
#12564=REPRESENTATION('material name',(#12583),#31630);
#12565=REPRESENTATION('density',(#12528),#31630);
#12566=REPRESENTATION('material name',(#12584),#31631);
#12567=REPRESENTATION('density',(#12529),#31631);
#12568=REPRESENTATION('material name',(#12585),#31632);
#12569=REPRESENTATION('density',(#12530),#31632);
#12570=REPRESENTATION('material name',(#12586),#31633);
#12571=REPRESENTATION('density',(#12531),#31633);
#12572=REPRESENTATION('material name',(#12587),#31634);
#12573=REPRESENTATION('density',(#12532),#31634);
#12574=REPRESENTATION('material name',(#12588),#31635);
#12575=REPRESENTATION('density',(#12533),#31635);
#12576=REPRESENTATION('material name',(#12589),#31636);
#12577=REPRESENTATION('density',(#12534),#31636);
#12578=REPRESENTATION('material name',(#12590),#31637);
#12579=REPRESENTATION('density',(#12535),#31637);
#12580=DESCRIPTIVE_REPRESENTATION_ITEM('Aluminum','Aluminum');
#12581=DESCRIPTIVE_REPRESENTATION_ITEM('Steel','Steel');
#12582=DESCRIPTIVE_REPRESENTATION_ITEM('Steel','Steel');
#12583=DESCRIPTIVE_REPRESENTATION_ITEM('Steel','Steel');
#12584=DESCRIPTIVE_REPRESENTATION_ITEM('Steel','Steel');
#12585=DESCRIPTIVE_REPRESENTATION_ITEM('Steel','Steel');
#12586=DESCRIPTIVE_REPRESENTATION_ITEM('Steel','Steel');
#12587=DESCRIPTIVE_REPRESENTATION_ITEM('Steel','Steel');
#12588=DESCRIPTIVE_REPRESENTATION_ITEM('Steel','Steel');
#12589=DESCRIPTIVE_REPRESENTATION_ITEM('Steel','Steel');
#12590=DESCRIPTIVE_REPRESENTATION_ITEM('Steel','Steel');
#12591=PROPERTY_DEFINITION('material property','material name',#31718);
#12592=PROPERTY_DEFINITION('material property','density of part',#31718);
#12593=PROPERTY_DEFINITION('material property','material name',#31719);
#12594=PROPERTY_DEFINITION('material property','density of part',#31719);
#12595=PROPERTY_DEFINITION('material property','material name',#31720);
#12596=PROPERTY_DEFINITION('material property','density of part',#31720);
#12597=PROPERTY_DEFINITION('material property','material name',#31721);
#12598=PROPERTY_DEFINITION('material property','density of part',#31721);
#12599=PROPERTY_DEFINITION('material property','material name',#31722);
#12600=PROPERTY_DEFINITION('material property','density of part',#31722);
#12601=PROPERTY_DEFINITION('material property','material name',#31723);
#12602=PROPERTY_DEFINITION('material property','density of part',#31723);
#12603=PROPERTY_DEFINITION('material property','material name',#31724);
#12604=PROPERTY_DEFINITION('material property','density of part',#31724);
#12605=PROPERTY_DEFINITION('material property','material name',#31725);
#12606=PROPERTY_DEFINITION('material property','density of part',#31725);
#12607=PROPERTY_DEFINITION('material property','material name',#31726);
#12608=PROPERTY_DEFINITION('material property','density of part',#31726);
#12609=PROPERTY_DEFINITION('material property','material name',#31727);
#12610=PROPERTY_DEFINITION('material property','density of part',#31727);
#12611=PROPERTY_DEFINITION('material property','material name',#31728);
#12612=PROPERTY_DEFINITION('material property','density of part',#31728);
#12613=AXIS2_PLACEMENT_3D('',#16339,#13620,#13621);
#12614=AXIS2_PLACEMENT_3D('',#16340,#13622,#13623);
#12615=AXIS2_PLACEMENT_3D('',#16341,#13624,#13625);
#12616=AXIS2_PLACEMENT_3D('',#16354,#13632,#13633);
#12617=AXIS2_PLACEMENT_3D('',#16358,#13635,#13636);
#12618=AXIS2_PLACEMENT_3D('',#16362,#13638,#13639);
#12619=AXIS2_PLACEMENT_3D('',#16365,#13641,#13642);
#12620=AXIS2_PLACEMENT_3D('',#16366,#13643,#13644);
#12621=AXIS2_PLACEMENT_3D('',#16372,#13648,#13649);
#12622=AXIS2_PLACEMENT_3D('',#16382,#13655,#13656);
#12623=AXIS2_PLACEMENT_3D('',#16392,#13662,#13663);
#12624=AXIS2_PLACEMENT_3D('',#16398,#13667,#13668);
#12625=AXIS2_PLACEMENT_3D('',#16406,#13673,#13674);
#12626=AXIS2_PLACEMENT_3D('',#16413,#13679,#13680);
#12627=AXIS2_PLACEMENT_3D('',#16421,#13685,#13686);
#12628=AXIS2_PLACEMENT_3D('',#16425,#13689,#13690);
#12629=AXIS2_PLACEMENT_3D('',#16435,#13696,#13697);
#12630=AXIS2_PLACEMENT_3D('',#16445,#13703,#13704);
#12631=AXIS2_PLACEMENT_3D('',#16452,#13708,#13709);
#12632=AXIS2_PLACEMENT_3D('',#16453,#13710,#13711);
#12633=AXIS2_PLACEMENT_3D('',#16461,#13716,#13717);
#12634=AXIS2_PLACEMENT_3D('',#16466,#13721,#13722);
#12635=AXIS2_PLACEMENT_3D('',#16474,#13727,#13728);
#12636=AXIS2_PLACEMENT_3D('',#16478,#13731,#13732);
#12637=AXIS2_PLACEMENT_3D('',#16488,#13738,#13739);
#12638=AXIS2_PLACEMENT_3D('',#16492,#13742,#13743);
#12639=AXIS2_PLACEMENT_3D('',#16500,#13748,#13749);
#12640=AXIS2_PLACEMENT_3D('',#16508,#13754,#13755);
#12641=AXIS2_PLACEMENT_3D('',#16521,#13762,#13763);
#12642=AXIS2_PLACEMENT_3D('',#16530,#13769,#13770);
#12643=AXIS2_PLACEMENT_3D('',#16538,#13775,#13776);
#12644=AXIS2_PLACEMENT_3D('',#16543,#13779,#13780);
#12645=AXIS2_PLACEMENT_3D('',#16544,#13781,#13782);
#12646=AXIS2_PLACEMENT_3D('',#16552,#13787,#13788);
#12647=AXIS2_PLACEMENT_3D('',#16554,#13790,#13791);
#12648=AXIS2_PLACEMENT_3D('',#16562,#13796,#13797);
#12649=AXIS2_PLACEMENT_3D('',#16567,#13801,#13802);
#12650=AXIS2_PLACEMENT_3D('',#16575,#13807,#13808);
#12651=AXIS2_PLACEMENT_3D('',#16585,#13814,#13815);
#12652=AXIS2_PLACEMENT_3D('',#16595,#13821,#13822);
#12653=AXIS2_PLACEMENT_3D('',#16601,#13826,#13827);
#12654=AXIS2_PLACEMENT_3D('',#16609,#13832,#13833);
#12655=AXIS2_PLACEMENT_3D('',#16616,#13838,#13839);
#12656=AXIS2_PLACEMENT_3D('',#16624,#13844,#13845);
#12657=AXIS2_PLACEMENT_3D('',#16628,#13848,#13849);
#12658=AXIS2_PLACEMENT_3D('',#16638,#13855,#13856);
#12659=AXIS2_PLACEMENT_3D('',#16648,#13862,#13863);
#12660=AXIS2_PLACEMENT_3D('',#16652,#13865,#13866);
#12661=AXIS2_PLACEMENT_3D('',#16656,#13868,#13869);
#12662=AXIS2_PLACEMENT_3D('',#16659,#13871,#13872);
#12663=AXIS2_PLACEMENT_3D('',#16660,#13873,#13874);
#12664=AXIS2_PLACEMENT_3D('',#16666,#13878,#13879);
#12665=AXIS2_PLACEMENT_3D('',#16671,#13883,#13884);
#12666=AXIS2_PLACEMENT_3D('',#16677,#13888,#13889);
#12667=AXIS2_PLACEMENT_3D('',#16738,#13893,#13894);
#12668=AXIS2_PLACEMENT_3D('',#16791,#13901,#13902);
#12669=AXIS2_PLACEMENT_3D('',#16793,#13903,#13904);
#12670=AXIS2_PLACEMENT_3D('',#16795,#13905,#13906);
#12671=AXIS2_PLACEMENT_3D('',#16797,#13907,#13908);
#12672=AXIS2_PLACEMENT_3D('',#16821,#13911,#13912);
#12673=AXIS2_PLACEMENT_3D('',#16824,#13915,#13916);
#12674=AXIS2_PLACEMENT_3D('',#16825,#13917,#13918);
#12675=AXIS2_PLACEMENT_3D('',#16828,#13921,#13922);
#12676=AXIS2_PLACEMENT_3D('',#16829,#13923,#13924);
#12677=AXIS2_PLACEMENT_3D('',#16876,#13926,#13927);
#12678=AXIS2_PLACEMENT_3D('',#16882,#13931,#13932);
#12679=AXIS2_PLACEMENT_3D('',#16943,#13936,#13937);
#12680=AXIS2_PLACEMENT_3D('',#16995,#13944,#13945);
#12681=AXIS2_PLACEMENT_3D('',#16997,#13946,#13947);
#12682=AXIS2_PLACEMENT_3D('',#16999,#13948,#13949);
#12683=AXIS2_PLACEMENT_3D('',#17001,#13950,#13951);
#12684=AXIS2_PLACEMENT_3D('',#17025,#13954,#13955);
#12685=AXIS2_PLACEMENT_3D('',#17030,#13959,#13960);
#12686=AXIS2_PLACEMENT_3D('',#17032,#13962,#13963);
#12687=AXIS2_PLACEMENT_3D('',#17033,#13964,#13965);
#12688=AXIS2_PLACEMENT_3D('',#17036,#13968,#13969);
#12689=AXIS2_PLACEMENT_3D('',#17038,#13971,#13972);
#12690=AXIS2_PLACEMENT_3D('',#17085,#13974,#13975);
#12691=AXIS2_PLACEMENT_3D('',#17088,#13977,#13978);
#12692=AXIS2_PLACEMENT_3D('',#17089,#13979,#13980);
#12693=AXIS2_PLACEMENT_3D('',#17091,#13981,#13982);
#12694=AXIS2_PLACEMENT_3D('',#17093,#13984,#13985);
#12695=AXIS2_PLACEMENT_3D('',#17095,#13987,#13988);
#12696=AXIS2_PLACEMENT_3D('',#17098,#13990,#13991);
#12697=AXIS2_PLACEMENT_3D('',#17099,#13992,#13993);
#12698=AXIS2_PLACEMENT_3D('',#17101,#13994,#13995);
#12699=AXIS2_PLACEMENT_3D('',#17103,#13997,#13998);
#12700=AXIS2_PLACEMENT_3D('',#17105,#14000,#14001);
#12701=AXIS2_PLACEMENT_3D('',#17108,#14003,#14004);
#12702=AXIS2_PLACEMENT_3D('',#17109,#14005,#14006);
#12703=AXIS2_PLACEMENT_3D('',#17111,#14007,#14008);
#12704=AXIS2_PLACEMENT_3D('',#17113,#14010,#14011);
#12705=AXIS2_PLACEMENT_3D('',#17115,#14013,#14014);
#12706=AXIS2_PLACEMENT_3D('',#17118,#14016,#14017);
#12707=AXIS2_PLACEMENT_3D('',#17119,#14018,#14019);
#12708=AXIS2_PLACEMENT_3D('',#17121,#14020,#14021);
#12709=AXIS2_PLACEMENT_3D('',#17123,#14023,#14024);
#12710=AXIS2_PLACEMENT_3D('',#17125,#14026,#14027);
#12711=AXIS2_PLACEMENT_3D('',#17127,#14028,#14029);
#12712=AXIS2_PLACEMENT_3D('',#17130,#14031,#14032);
#12713=AXIS2_PLACEMENT_3D('',#17131,#14033,#14034);
#12714=AXIS2_PLACEMENT_3D('',#17134,#14036,#14037);
#12715=AXIS2_PLACEMENT_3D('',#17135,#14038,#14039);
#12716=AXIS2_PLACEMENT_3D('',#17137,#14040,#14041);
#12717=AXIS2_PLACEMENT_3D('',#17138,#14042,#14043);
#12718=AXIS2_PLACEMENT_3D('',#17141,#14045,#14046);
#12719=AXIS2_PLACEMENT_3D('',#17142,#14047,#14048);
#12720=AXIS2_PLACEMENT_3D('',#17144,#14049,#14050);
#12721=AXIS2_PLACEMENT_3D('',#17145,#14051,#14052);
#12722=AXIS2_PLACEMENT_3D('',#17148,#14054,#14055);
#12723=AXIS2_PLACEMENT_3D('',#17149,#14056,#14057);
#12724=AXIS2_PLACEMENT_3D('',#17152,#14059,#14060);
#12725=AXIS2_PLACEMENT_3D('',#17153,#14061,#14062);
#12726=AXIS2_PLACEMENT_3D('',#17156,#14064,#14065);
#12727=AXIS2_PLACEMENT_3D('',#17157,#14066,#14067);
#12728=AXIS2_PLACEMENT_3D('',#17160,#14069,#14070);
#12729=AXIS2_PLACEMENT_3D('',#17161,#14071,#14072);
#12730=AXIS2_PLACEMENT_3D('',#17163,#14073,#14074);
#12731=AXIS2_PLACEMENT_3D('',#17164,#14075,#14076);
#12732=AXIS2_PLACEMENT_3D('',#17167,#14078,#14079);
#12733=AXIS2_PLACEMENT_3D('',#17168,#14080,#14081);
#12734=AXIS2_PLACEMENT_3D('',#17170,#14082,#14083);
#12735=AXIS2_PLACEMENT_3D('',#17171,#14084,#14085);
#12736=AXIS2_PLACEMENT_3D('',#17174,#14087,#14088);
#12737=AXIS2_PLACEMENT_3D('',#17175,#14089,#14090);
#12738=AXIS2_PLACEMENT_3D('',#17177,#14092,#14093);
#12739=AXIS2_PLACEMENT_3D('',#17180,#14095,#14096);
#12740=AXIS2_PLACEMENT_3D('',#17181,#14097,#14098);
#12741=AXIS2_PLACEMENT_3D('',#17184,#14100,#14101);
#12742=AXIS2_PLACEMENT_3D('',#17185,#14102,#14103);
#12743=AXIS2_PLACEMENT_3D('',#17187,#14104,#14105);
#12744=AXIS2_PLACEMENT_3D('',#17188,#14106,#14107);
#12745=AXIS2_PLACEMENT_3D('',#17191,#14109,#14110);
#12746=AXIS2_PLACEMENT_3D('',#17192,#14111,#14112);
#12747=AXIS2_PLACEMENT_3D('',#17194,#14113,#14114);
#12748=AXIS2_PLACEMENT_3D('',#17195,#14115,#14116);
#12749=AXIS2_PLACEMENT_3D('',#17198,#14118,#14119);
#12750=AXIS2_PLACEMENT_3D('',#17199,#14120,#14121);
#12751=AXIS2_PLACEMENT_3D('',#17296,#14123,#14124);
#12752=AXIS2_PLACEMENT_3D('',#17297,#14125,#14126);
#12753=AXIS2_PLACEMENT_3D('',#17298,#14127,#14128);
#12754=AXIS2_PLACEMENT_3D('',#17299,#14129,#14130);
#12755=AXIS2_PLACEMENT_3D('',#17300,#14131,#14132);
#12756=AXIS2_PLACEMENT_3D('',#17301,#14133,#14134);
#12757=AXIS2_PLACEMENT_3D('',#17302,#14135,#14136);
#12758=AXIS2_PLACEMENT_3D('',#17527,#14139,#14140);
#12759=AXIS2_PLACEMENT_3D('',#17529,#14141,#14142);
#12760=AXIS2_PLACEMENT_3D('',#17530,#14143,#14144);
#12761=AXIS2_PLACEMENT_3D('',#17531,#14145,#14146);
#12762=AXIS2_PLACEMENT_3D('',#17533,#14147,#14148);
#12763=AXIS2_PLACEMENT_3D('',#17534,#14149,#14150);
#12764=AXIS2_PLACEMENT_3D('',#17535,#14151,#14152);
#12765=AXIS2_PLACEMENT_3D('',#17536,#14153,#14154);
#12766=AXIS2_PLACEMENT_3D('',#17538,#14155,#14156);
#12767=AXIS2_PLACEMENT_3D('',#17539,#14157,#14158);
#12768=AXIS2_PLACEMENT_3D('',#17540,#14159,#14160);
#12769=AXIS2_PLACEMENT_3D('',#17542,#14161,#14162);
#12770=AXIS2_PLACEMENT_3D('',#17544,#14164,#14165);
#12771=AXIS2_PLACEMENT_3D('',#17545,#14166,#14167);
#12772=AXIS2_PLACEMENT_3D('',#17546,#14168,#14169);
#12773=AXIS2_PLACEMENT_3D('',#17548,#14171,#14172);
#12774=AXIS2_PLACEMENT_3D('',#17550,#14174,#14175);
#12775=AXIS2_PLACEMENT_3D('',#17552,#14177,#14178);
#12776=AXIS2_PLACEMENT_3D('',#17553,#14179,#14180);
#12777=AXIS2_PLACEMENT_3D('',#17554,#14181,#14182);
#12778=AXIS2_PLACEMENT_3D('',#17556,#14183,#14184);
#12779=AXIS2_PLACEMENT_3D('',#17560,#14186,#14187);
#12780=AXIS2_PLACEMENT_3D('',#17561,#14188,#14189);
#12781=AXIS2_PLACEMENT_3D('',#17562,#14190,#14191);
#12782=AXIS2_PLACEMENT_3D('',#17590,#14193,#14194);
#12783=AXIS2_PLACEMENT_3D('',#17616,#14195,#14196);
#12784=AXIS2_PLACEMENT_3D('',#17642,#14197,#14198);
#12785=AXIS2_PLACEMENT_3D('',#17668,#14199,#14200);
#12786=AXIS2_PLACEMENT_3D('',#17694,#14201,#14202);
#12787=AXIS2_PLACEMENT_3D('',#17720,#14203,#14204);
#12788=AXIS2_PLACEMENT_3D('',#17746,#14205,#14206);
#12789=AXIS2_PLACEMENT_3D('',#17772,#14207,#14208);
#12790=AXIS2_PLACEMENT_3D('',#17798,#14209,#14210);
#12791=AXIS2_PLACEMENT_3D('',#17824,#14211,#14212);
#12792=AXIS2_PLACEMENT_3D('',#17850,#14213,#14214);
#12793=AXIS2_PLACEMENT_3D('',#17876,#14215,#14216);
#12794=AXIS2_PLACEMENT_3D('',#17902,#14217,#14218);
#12795=AXIS2_PLACEMENT_3D('',#17928,#14219,#14220);
#12796=AXIS2_PLACEMENT_3D('',#17954,#14221,#14222);
#12797=AXIS2_PLACEMENT_3D('',#17980,#14223,#14224);
#12798=AXIS2_PLACEMENT_3D('',#18006,#14225,#14226);
#12799=AXIS2_PLACEMENT_3D('',#18032,#14227,#14228);
#12800=AXIS2_PLACEMENT_3D('',#18058,#14229,#14230);
#12801=AXIS2_PLACEMENT_3D('',#18084,#14231,#14232);
#12802=AXIS2_PLACEMENT_3D('',#18089,#14233,#14234);
#12803=AXIS2_PLACEMENT_3D('',#18092,#14235,#14236);
#12804=AXIS2_PLACEMENT_3D('',#18132,#14237,#14238);
#12805=AXIS2_PLACEMENT_3D('',#18379,#14239,#14240);
#12806=AXIS2_PLACEMENT_3D('',#18381,#14241,#14242);
#12807=AXIS2_PLACEMENT_3D('',#18383,#14243,#14244);
#12808=AXIS2_PLACEMENT_3D('',#18396,#14245,#14246);
#12809=AXIS2_PLACEMENT_3D('',#18412,#14247,#14248);
#12810=AXIS2_PLACEMENT_3D('',#18413,#14249,#14250);
#12811=AXIS2_PLACEMENT_3D('',#18630,#14252,#14253);
#12812=AXIS2_PLACEMENT_3D('',#18670,#14255,#14256);
#12813=AXIS2_PLACEMENT_3D('',#18672,#14257,#14258);
#12814=AXIS2_PLACEMENT_3D('',#18791,#14260,#14261);
#12815=AXIS2_PLACEMENT_3D('',#18793,#14262,#14263);
#12816=AXIS2_PLACEMENT_3D('',#18802,#14264,#14265);
#12817=AXIS2_PLACEMENT_3D('',#18812,#14266,#14267);
#12818=AXIS2_PLACEMENT_3D('',#18921,#14268,#14269);
#12819=AXIS2_PLACEMENT_3D('',#18931,#14270,#14271);
#12820=AXIS2_PLACEMENT_3D('',#19040,#14272,#14273);
#12821=AXIS2_PLACEMENT_3D('',#19050,#14274,#14275);
#12822=AXIS2_PLACEMENT_3D('',#19159,#14276,#14277);
#12823=AXIS2_PLACEMENT_3D('',#19169,#14278,#14279);
#12824=AXIS2_PLACEMENT_3D('',#19278,#14280,#14281);
#12825=AXIS2_PLACEMENT_3D('',#19288,#14282,#14283);
#12826=AXIS2_PLACEMENT_3D('',#19397,#14284,#14285);
#12827=AXIS2_PLACEMENT_3D('',#19407,#14286,#14287);
#12828=AXIS2_PLACEMENT_3D('',#19516,#14288,#14289);
#12829=AXIS2_PLACEMENT_3D('',#19526,#14290,#14291);
#12830=AXIS2_PLACEMENT_3D('',#19635,#14292,#14293);
#12831=AXIS2_PLACEMENT_3D('',#19645,#14294,#14295);
#12832=AXIS2_PLACEMENT_3D('',#19754,#14296,#14297);
#12833=AXIS2_PLACEMENT_3D('',#19764,#14298,#14299);
#12834=AXIS2_PLACEMENT_3D('',#19878,#14300,#14301);
#12835=AXIS2_PLACEMENT_3D('',#19888,#14302,#14303);
#12836=AXIS2_PLACEMENT_3D('',#19997,#14304,#14305);
#12837=AXIS2_PLACEMENT_3D('',#20007,#14306,#14307);
#12838=AXIS2_PLACEMENT_3D('',#20116,#14308,#14309);
#12839=AXIS2_PLACEMENT_3D('',#20126,#14310,#14311);
#12840=AXIS2_PLACEMENT_3D('',#20235,#14312,#14313);
#12841=AXIS2_PLACEMENT_3D('',#20245,#14314,#14315);
#12842=AXIS2_PLACEMENT_3D('',#20354,#14316,#14317);
#12843=AXIS2_PLACEMENT_3D('',#20364,#14318,#14319);
#12844=AXIS2_PLACEMENT_3D('',#20473,#14320,#14321);
#12845=AXIS2_PLACEMENT_3D('',#20483,#14322,#14323);
#12846=AXIS2_PLACEMENT_3D('',#20592,#14324,#14325);
#12847=AXIS2_PLACEMENT_3D('',#20602,#14326,#14327);
#12848=AXIS2_PLACEMENT_3D('',#20711,#14328,#14329);
#12849=AXIS2_PLACEMENT_3D('',#20721,#14330,#14331);
#12850=AXIS2_PLACEMENT_3D('',#20830,#14332,#14333);
#12851=AXIS2_PLACEMENT_3D('',#20840,#14334,#14335);
#12852=AXIS2_PLACEMENT_3D('',#21057,#14336,#14337);
#12853=AXIS2_PLACEMENT_3D('',#21059,#14338,#14339);
#12854=AXIS2_PLACEMENT_3D('',#21061,#14341,#14342);
#12855=AXIS2_PLACEMENT_3D('',#21062,#14343,#14344);
#12856=AXIS2_PLACEMENT_3D('',#21063,#14345,#14346);
#12857=AXIS2_PLACEMENT_3D('',#21065,#14347,#14348);
#12858=AXIS2_PLACEMENT_3D('',#21066,#14349,#14350);
#12859=AXIS2_PLACEMENT_3D('',#21069,#14352,#14353);
#12860=AXIS2_PLACEMENT_3D('',#21070,#14354,#14355);
#12861=AXIS2_PLACEMENT_3D('',#21073,#14357,#14358);
#12862=AXIS2_PLACEMENT_3D('',#21074,#14359,#14360);
#12863=AXIS2_PLACEMENT_3D('',#21077,#14362,#14363);
#12864=AXIS2_PLACEMENT_3D('',#21078,#14364,#14365);
#12865=AXIS2_PLACEMENT_3D('',#21079,#14366,#14367);
#12866=AXIS2_PLACEMENT_3D('',#21080,#14368,#14369);
#12867=AXIS2_PLACEMENT_3D('',#21082,#14370,#14371);
#12868=AXIS2_PLACEMENT_3D('',#21086,#14373,#14374);
#12869=AXIS2_PLACEMENT_3D('',#21087,#14375,#14376);
#12870=AXIS2_PLACEMENT_3D('',#21088,#14377,#14378);
#12871=AXIS2_PLACEMENT_3D('',#21090,#14379,#14380);
#12872=AXIS2_PLACEMENT_3D('',#21092,#14382,#14383);
#12873=AXIS2_PLACEMENT_3D('',#21094,#14384,#14385);
#12874=AXIS2_PLACEMENT_3D('',#21095,#14386,#14387);
#12875=AXIS2_PLACEMENT_3D('',#21098,#14389,#14390);
#12876=AXIS2_PLACEMENT_3D('',#21101,#14391,#14392);
#12877=AXIS2_PLACEMENT_3D('',#21103,#14394,#14395);
#12878=AXIS2_PLACEMENT_3D('',#21106,#14396,#14397);
#12879=AXIS2_PLACEMENT_3D('',#21108,#14399,#14400);
#12880=AXIS2_PLACEMENT_3D('',#21111,#14403,#14404);
#12881=AXIS2_PLACEMENT_3D('',#21114,#14405,#14406);
#12882=AXIS2_PLACEMENT_3D('',#21116,#14408,#14409);
#12883=AXIS2_PLACEMENT_3D('',#21122,#14413,#14414);
#12884=AXIS2_PLACEMENT_3D('',#21123,#14415,#14416);
#12885=AXIS2_PLACEMENT_3D('',#21124,#14417,#14418);
#12886=AXIS2_PLACEMENT_3D('',#21126,#14419,#14420);
#12887=AXIS2_PLACEMENT_3D('',#21127,#14421,#14422);
#12888=AXIS2_PLACEMENT_3D('',#21129,#14423,#14424);
#12889=AXIS2_PLACEMENT_3D('',#21131,#14426,#14427);
#12890=AXIS2_PLACEMENT_3D('',#21133,#14428,#14429);
#12891=AXIS2_PLACEMENT_3D('',#21135,#14431,#14432);
#12892=AXIS2_PLACEMENT_3D('',#21137,#14433,#14434);
#12893=AXIS2_PLACEMENT_3D('',#21138,#14435,#14436);
#12894=AXIS2_PLACEMENT_3D('',#21140,#14437,#14438);
#12895=AXIS2_PLACEMENT_3D('',#21142,#14440,#14441);
#12896=AXIS2_PLACEMENT_3D('',#21144,#14442,#14443);
#12897=AXIS2_PLACEMENT_3D('',#21145,#14444,#14445);
#12898=AXIS2_PLACEMENT_3D('',#21147,#14446,#14447);
#12899=AXIS2_PLACEMENT_3D('',#21149,#14449,#14450);
#12900=AXIS2_PLACEMENT_3D('',#21151,#14452,#14453);
#12901=AXIS2_PLACEMENT_3D('',#21400,#14454,#14455);
#12902=AXIS2_PLACEMENT_3D('',#21402,#14456,#14457);
#12903=AXIS2_PLACEMENT_3D('',#21404,#14458,#14459);
#12904=AXIS2_PLACEMENT_3D('',#21418,#14460,#14461);
#12905=AXIS2_PLACEMENT_3D('',#21419,#14462,#14463);
#12906=AXIS2_PLACEMENT_3D('',#21421,#14464,#14465);
#12907=AXIS2_PLACEMENT_3D('',#21437,#14466,#14467);
#12908=AXIS2_PLACEMENT_3D('',#21438,#14468,#14469);
#12909=AXIS2_PLACEMENT_3D('',#21692,#14471,#14472);
#12910=AXIS2_PLACEMENT_3D('',#21732,#14474,#14475);
#12911=AXIS2_PLACEMENT_3D('',#21734,#14476,#14477);
#12912=AXIS2_PLACEMENT_3D('',#21878,#14479,#14480);
#12913=AXIS2_PLACEMENT_3D('',#21880,#14481,#14482);
#12914=AXIS2_PLACEMENT_3D('',#21889,#14484,#14485);
#12915=AXIS2_PLACEMENT_3D('',#21915,#14486,#14487);
#12916=AXIS2_PLACEMENT_3D('',#21941,#14488,#14489);
#12917=AXIS2_PLACEMENT_3D('',#21967,#14490,#14491);
#12918=AXIS2_PLACEMENT_3D('',#21993,#14492,#14493);
#12919=AXIS2_PLACEMENT_3D('',#22019,#14494,#14495);
#12920=AXIS2_PLACEMENT_3D('',#22045,#14496,#14497);
#12921=AXIS2_PLACEMENT_3D('',#22071,#14498,#14499);
#12922=AXIS2_PLACEMENT_3D('',#22097,#14500,#14501);
#12923=AXIS2_PLACEMENT_3D('',#22122,#14502,#14503);
#12924=AXIS2_PLACEMENT_3D('',#22124,#14504,#14505);
#12925=AXIS2_PLACEMENT_3D('',#22150,#14506,#14507);
#12926=AXIS2_PLACEMENT_3D('',#22176,#14508,#14509);
#12927=AXIS2_PLACEMENT_3D('',#22202,#14510,#14511);
#12928=AXIS2_PLACEMENT_3D('',#22228,#14512,#14513);
#12929=AXIS2_PLACEMENT_3D('',#22254,#14514,#14515);
#12930=AXIS2_PLACEMENT_3D('',#22280,#14516,#14517);
#12931=AXIS2_PLACEMENT_3D('',#22306,#14518,#14519);
#12932=AXIS2_PLACEMENT_3D('',#22332,#14520,#14521);
#12933=AXIS2_PLACEMENT_3D('',#22358,#14522,#14523);
#12934=AXIS2_PLACEMENT_3D('',#22382,#14524,#14525);
#12935=AXIS2_PLACEMENT_3D('',#22384,#14526,#14527);
#12936=AXIS2_PLACEMENT_3D('',#22393,#14528,#14529);
#12937=AXIS2_PLACEMENT_3D('',#22403,#14530,#14531);
#12938=AXIS2_PLACEMENT_3D('',#22512,#14532,#14533);
#12939=AXIS2_PLACEMENT_3D('',#22522,#14534,#14535);
#12940=AXIS2_PLACEMENT_3D('',#22631,#14536,#14537);
#12941=AXIS2_PLACEMENT_3D('',#22641,#14538,#14539);
#12942=AXIS2_PLACEMENT_3D('',#22750,#14540,#14541);
#12943=AXIS2_PLACEMENT_3D('',#22760,#14542,#14543);
#12944=AXIS2_PLACEMENT_3D('',#22869,#14544,#14545);
#12945=AXIS2_PLACEMENT_3D('',#22879,#14546,#14547);
#12946=AXIS2_PLACEMENT_3D('',#22988,#14548,#14549);
#12947=AXIS2_PLACEMENT_3D('',#22998,#14550,#14551);
#12948=AXIS2_PLACEMENT_3D('',#23107,#14552,#14553);
#12949=AXIS2_PLACEMENT_3D('',#23117,#14554,#14555);
#12950=AXIS2_PLACEMENT_3D('',#23226,#14556,#14557);
#12951=AXIS2_PLACEMENT_3D('',#23236,#14558,#14559);
#12952=AXIS2_PLACEMENT_3D('',#23345,#14560,#14561);
#12953=AXIS2_PLACEMENT_3D('',#23355,#14562,#14563);
#12954=AXIS2_PLACEMENT_3D('',#23469,#14564,#14565);
#12955=AXIS2_PLACEMENT_3D('',#23479,#14566,#14567);
#12956=AXIS2_PLACEMENT_3D('',#23588,#14568,#14569);
#12957=AXIS2_PLACEMENT_3D('',#23598,#14570,#14571);
#12958=AXIS2_PLACEMENT_3D('',#23707,#14572,#14573);
#12959=AXIS2_PLACEMENT_3D('',#23717,#14574,#14575);
#12960=AXIS2_PLACEMENT_3D('',#23826,#14576,#14577);
#12961=AXIS2_PLACEMENT_3D('',#23836,#14578,#14579);
#12962=AXIS2_PLACEMENT_3D('',#23945,#14580,#14581);
#12963=AXIS2_PLACEMENT_3D('',#23955,#14582,#14583);
#12964=AXIS2_PLACEMENT_3D('',#24064,#14584,#14585);
#12965=AXIS2_PLACEMENT_3D('',#24074,#14586,#14587);
#12966=AXIS2_PLACEMENT_3D('',#24183,#14588,#14589);
#12967=AXIS2_PLACEMENT_3D('',#24193,#14590,#14591);
#12968=AXIS2_PLACEMENT_3D('',#24302,#14592,#14593);
#12969=AXIS2_PLACEMENT_3D('',#24312,#14594,#14595);
#12970=AXIS2_PLACEMENT_3D('',#24421,#14596,#14597);
#12971=AXIS2_PLACEMENT_3D('',#24431,#14598,#14599);
#12972=AXIS2_PLACEMENT_3D('',#24648,#14600,#14601);
#12973=AXIS2_PLACEMENT_3D('',#24650,#14602,#14603);
#12974=AXIS2_PLACEMENT_3D('',#24652,#14605,#14606);
#12975=AXIS2_PLACEMENT_3D('',#24653,#14607,#14608);
#12976=AXIS2_PLACEMENT_3D('',#24654,#14609,#14610);
#12977=AXIS2_PLACEMENT_3D('',#24655,#14611,#14612);
#12978=AXIS2_PLACEMENT_3D('',#24657,#14613,#14614);
#12979=AXIS2_PLACEMENT_3D('',#24658,#14615,#14616);
#12980=AXIS2_PLACEMENT_3D('',#24661,#14618,#14619);
#12981=AXIS2_PLACEMENT_3D('',#24662,#14620,#14621);
#12982=AXIS2_PLACEMENT_3D('',#24665,#14623,#14624);
#12983=AXIS2_PLACEMENT_3D('',#24666,#14625,#14626);
#12984=AXIS2_PLACEMENT_3D('',#24669,#14628,#14629);
#12985=AXIS2_PLACEMENT_3D('',#24670,#14630,#14631);
#12986=AXIS2_PLACEMENT_3D('',#24671,#14632,#14633);
#12987=AXIS2_PLACEMENT_3D('',#24672,#14634,#14635);
#12988=AXIS2_PLACEMENT_3D('',#24674,#14636,#14637);
#12989=AXIS2_PLACEMENT_3D('',#24676,#14638,#14639);
#12990=AXIS2_PLACEMENT_3D('',#24677,#14640,#14641);
#12991=AXIS2_PLACEMENT_3D('',#24679,#14642,#14643);
#12992=AXIS2_PLACEMENT_3D('',#24681,#14644,#14645);
#12993=AXIS2_PLACEMENT_3D('',#24682,#14646,#14647);
#12994=AXIS2_PLACEMENT_3D('',#24684,#14649,#14650);
#12995=AXIS2_PLACEMENT_3D('',#24686,#14651,#14652);
#12996=AXIS2_PLACEMENT_3D('',#24688,#14654,#14655);
#12997=AXIS2_PLACEMENT_3D('',#24690,#14656,#14657);
#12998=AXIS2_PLACEMENT_3D('',#24692,#14658,#14659);
#12999=AXIS2_PLACEMENT_3D('',#24693,#14660,#14661);
#13000=AXIS2_PLACEMENT_3D('',#24695,#14662,#14663);
#13001=AXIS2_PLACEMENT_3D('',#24697,#14664,#14665);
#13002=AXIS2_PLACEMENT_3D('',#24698,#14666,#14667);
#13003=AXIS2_PLACEMENT_3D('',#24700,#14669,#14670);
#13004=AXIS2_PLACEMENT_3D('',#24710,#14671,#14672);
#13005=AXIS2_PLACEMENT_3D('',#24719,#14673,#14674);
#13006=AXIS2_PLACEMENT_3D('',#24728,#14675,#14676);
#13007=AXIS2_PLACEMENT_3D('',#24737,#14677,#14678);
#13008=AXIS2_PLACEMENT_3D('',#24746,#14679,#14680);
#13009=AXIS2_PLACEMENT_3D('',#24749,#14682,#14683);
#13010=AXIS2_PLACEMENT_3D('',#24758,#14684,#14685);
#13011=AXIS2_PLACEMENT_3D('',#24766,#14686,#14687);
#13012=AXIS2_PLACEMENT_3D('',#24767,#14688,#14689);
#13013=AXIS2_PLACEMENT_3D('',#24803,#14690,#14691);
#13014=AXIS2_PLACEMENT_3D('',#24837,#14692,#14693);
#13015=AXIS2_PLACEMENT_3D('',#24892,#14694,#14695);
#13016=AXIS2_PLACEMENT_3D('',#24896,#14697,#14698);
#13017=AXIS2_PLACEMENT_3D('',#24905,#14699,#14700);
#13018=AXIS2_PLACEMENT_3D('',#24914,#14701,#14702);
#13019=AXIS2_PLACEMENT_3D('',#24923,#14703,#14704);
#13020=AXIS2_PLACEMENT_3D('',#24931,#14705,#14706);
#13021=AXIS2_PLACEMENT_3D('',#24933,#14707,#14708);
#13022=AXIS2_PLACEMENT_3D('',#24942,#14709,#14710);
#13023=AXIS2_PLACEMENT_3D('',#24950,#14711,#14712);
#13024=AXIS2_PLACEMENT_3D('',#24951,#14713,#14714);
#13025=AXIS2_PLACEMENT_3D('',#24975,#14715,#14716);
#13026=AXIS2_PLACEMENT_3D('',#24977,#14717,#14718);
#13027=AXIS2_PLACEMENT_3D('',#24989,#14719,#14720);
#13028=AXIS2_PLACEMENT_3D('',#25001,#14721,#14722);
#13029=AXIS2_PLACEMENT_3D('',#25004,#14724,#14725);
#13030=AXIS2_PLACEMENT_3D('',#25006,#14726,#14727);
#13031=AXIS2_PLACEMENT_3D('',#25018,#14728,#14729);
#13032=AXIS2_PLACEMENT_3D('',#25030,#14730,#14731);
#13033=AXIS2_PLACEMENT_3D('',#25042,#14732,#14733);
#13034=AXIS2_PLACEMENT_3D('',#25053,#14734,#14735);
#13035=AXIS2_PLACEMENT_3D('',#25054,#14736,#14737);
#13036=AXIS2_PLACEMENT_3D('',#25056,#14738,#14739);
#13037=AXIS2_PLACEMENT_3D('',#25079,#14740,#14741);
#13038=AXIS2_PLACEMENT_3D('',#25109,#14742,#14743);
#13039=AXIS2_PLACEMENT_3D('',#25115,#14744,#14745);
#13040=AXIS2_PLACEMENT_3D('',#25139,#14746,#14747);
#13041=AXIS2_PLACEMENT_3D('',#25163,#14748,#14749);
#13042=AXIS2_PLACEMENT_3D('',#25165,#14750,#14751);
#13043=AXIS2_PLACEMENT_3D('',#25188,#14752,#14753);
#13044=AXIS2_PLACEMENT_3D('',#25218,#14754,#14755);
#13045=AXIS2_PLACEMENT_3D('',#25224,#14756,#14757);
#13046=AXIS2_PLACEMENT_3D('',#25248,#14758,#14759);
#13047=AXIS2_PLACEMENT_3D('',#25272,#14760,#14761);
#13048=AXIS2_PLACEMENT_3D('',#25274,#14762,#14763);
#13049=AXIS2_PLACEMENT_3D('',#25276,#14764,#14765);
#13050=AXIS2_PLACEMENT_3D('',#25299,#14766,#14767);
#13051=AXIS2_PLACEMENT_3D('',#25329,#14768,#14769);
#13052=AXIS2_PLACEMENT_3D('',#25335,#14770,#14771);
#13053=AXIS2_PLACEMENT_3D('',#25359,#14772,#14773);
#13054=AXIS2_PLACEMENT_3D('',#25383,#14774,#14775);
#13055=AXIS2_PLACEMENT_3D('',#25385,#14776,#14777);
#13056=AXIS2_PLACEMENT_3D('',#25408,#14778,#14779);
#13057=AXIS2_PLACEMENT_3D('',#25438,#14780,#14781);
#13058=AXIS2_PLACEMENT_3D('',#25444,#14782,#14783);
#13059=AXIS2_PLACEMENT_3D('',#25468,#14784,#14785);
#13060=AXIS2_PLACEMENT_3D('',#25492,#14786,#14787);
#13061=AXIS2_PLACEMENT_3D('',#25494,#14788,#14789);
#13062=AXIS2_PLACEMENT_3D('',#25517,#14790,#14791);
#13063=AXIS2_PLACEMENT_3D('',#25524,#14792,#14793);
#13064=AXIS2_PLACEMENT_3D('',#25553,#14794,#14795);
#13065=AXIS2_PLACEMENT_3D('',#25577,#14796,#14797);
#13066=AXIS2_PLACEMENT_3D('',#25580,#14799,#14800);
#13067=AXIS2_PLACEMENT_3D('',#25581,#14801,#14802);
#13068=AXIS2_PLACEMENT_3D('',#25605,#14803,#14804);
#13069=AXIS2_PLACEMENT_3D('',#25607,#14805,#14806);
#13070=AXIS2_PLACEMENT_3D('',#25610,#14808,#14809);
#13071=AXIS2_PLACEMENT_3D('',#25621,#14810,#14811);
#13072=AXIS2_PLACEMENT_3D('',#25622,#14812,#14813);
#13073=AXIS2_PLACEMENT_3D('',#25645,#14814,#14815);
#13074=AXIS2_PLACEMENT_3D('',#25647,#14816,#14817);
#13075=AXIS2_PLACEMENT_3D('',#25671,#14818,#14819);
#13076=AXIS2_PLACEMENT_3D('',#25695,#14820,#14821);
#13077=AXIS2_PLACEMENT_3D('',#25696,#14822,#14823);
#13078=AXIS2_PLACEMENT_3D('',#25698,#14824,#14825);
#13079=AXIS2_PLACEMENT_3D('',#25699,#14826,#14827);
#13080=AXIS2_PLACEMENT_3D('',#25701,#14828,#14829);
#13081=AXIS2_PLACEMENT_3D('',#25703,#14831,#14832);
#13082=AXIS2_PLACEMENT_3D('',#25705,#14833,#14834);
#13083=AXIS2_PLACEMENT_3D('',#25707,#14836,#14837);
#13084=AXIS2_PLACEMENT_3D('',#25709,#14838,#14839);
#13085=AXIS2_PLACEMENT_3D('',#25711,#14841,#14842);
#13086=AXIS2_PLACEMENT_3D('',#25712,#14843,#14844);
#13087=AXIS2_PLACEMENT_3D('',#25713,#14845,#14846);
#13088=AXIS2_PLACEMENT_3D('',#25715,#14847,#14848);
#13089=AXIS2_PLACEMENT_3D('',#25718,#14850,#14851);
#13090=AXIS2_PLACEMENT_3D('',#25719,#14852,#14853);
#13091=AXIS2_PLACEMENT_3D('',#25722,#14855,#14856);
#13092=AXIS2_PLACEMENT_3D('',#25723,#14857,#14858);
#13093=AXIS2_PLACEMENT_3D('',#25724,#14859,#14860);
#13094=AXIS2_PLACEMENT_3D('',#25726,#14861,#14862);
#13095=AXIS2_PLACEMENT_3D('',#25727,#14863,#14864);
#13096=AXIS2_PLACEMENT_3D('',#25729,#14866,#14867);
#13097=AXIS2_PLACEMENT_3D('',#25730,#14868,#14869);
#13098=AXIS2_PLACEMENT_3D('',#25732,#14870,#14871);
#13099=AXIS2_PLACEMENT_3D('',#25735,#14873,#14874);
#13100=AXIS2_PLACEMENT_3D('',#25736,#14875,#14876);
#13101=AXIS2_PLACEMENT_3D('',#25738,#14877,#14878);
#13102=AXIS2_PLACEMENT_3D('',#25739,#14879,#14880);
#13103=AXIS2_PLACEMENT_3D('',#25741,#14881,#14882);
#13104=AXIS2_PLACEMENT_3D('',#25743,#14884,#14885);
#13105=AXIS2_PLACEMENT_3D('',#25744,#14886,#14887);
#13106=AXIS2_PLACEMENT_3D('',#25745,#14888,#14889);
#13107=AXIS2_PLACEMENT_3D('',#25752,#14892,#14893);
#13108=AXIS2_PLACEMENT_3D('',#25754,#14895,#14896);
#13109=AXIS2_PLACEMENT_3D('',#25760,#14900,#14901);
#13110=AXIS2_PLACEMENT_3D('',#25768,#14906,#14907);
#13111=AXIS2_PLACEMENT_3D('',#25775,#14910,#14911);
#13112=AXIS2_PLACEMENT_3D('',#25777,#14913,#14914);
#13113=AXIS2_PLACEMENT_3D('',#25783,#14918,#14919);
#13114=AXIS2_PLACEMENT_3D('',#25785,#14920,#14921);
#13115=AXIS2_PLACEMENT_3D('',#25787,#14922,#14923);
#13116=AXIS2_PLACEMENT_3D('',#25788,#14924,#14925);
#13117=AXIS2_PLACEMENT_3D('',#25789,#14926,#14927);
#13118=AXIS2_PLACEMENT_3D('',#25790,#14928,#14929);
#13119=AXIS2_PLACEMENT_3D('',#25792,#14931,#14932);
#13120=AXIS2_PLACEMENT_3D('',#25798,#14935,#14936);
#13121=AXIS2_PLACEMENT_3D('',#25807,#14941,#14942);
#13122=AXIS2_PLACEMENT_3D('',#25809,#14943,#14944);
#13123=AXIS2_PLACEMENT_3D('',#25810,#14945,#14946);
#13124=AXIS2_PLACEMENT_3D('',#25812,#14948,#14949);
#13125=AXIS2_PLACEMENT_3D('',#25816,#14952,#14953);
#13126=AXIS2_PLACEMENT_3D('',#25818,#14954,#14955);
#13127=AXIS2_PLACEMENT_3D('',#25820,#14957,#14958);
#13128=AXIS2_PLACEMENT_3D('',#25822,#14959,#14960);
#13129=AXIS2_PLACEMENT_3D('',#25824,#14962,#14963);
#13130=AXIS2_PLACEMENT_3D('',#25830,#14967,#14968);
#13131=AXIS2_PLACEMENT_3D('',#25832,#14970,#14971);
#13132=AXIS2_PLACEMENT_3D('',#25838,#14975,#14976);
#13133=AXIS2_PLACEMENT_3D('',#25840,#14978,#14979);
#13134=AXIS2_PLACEMENT_3D('',#25841,#14980,#14981);
#13135=AXIS2_PLACEMENT_3D('',#25842,#14982,#14983);
#13136=AXIS2_PLACEMENT_3D('',#25843,#14984,#14985);
#13137=AXIS2_PLACEMENT_3D('',#25844,#14986,#14987);
#13138=AXIS2_PLACEMENT_3D('',#25860,#14989,#14990);
#13139=AXIS2_PLACEMENT_3D('',#25868,#14991,#14992);
#13140=AXIS2_PLACEMENT_3D('',#25916,#14994,#14995);
#13141=AXIS2_PLACEMENT_3D('',#25964,#14997,#14998);
#13142=AXIS2_PLACEMENT_3D('',#26018,#15000,#15001);
#13143=AXIS2_PLACEMENT_3D('',#26066,#15003,#15004);
#13144=AXIS2_PLACEMENT_3D('',#26120,#15006,#15007);
#13145=AXIS2_PLACEMENT_3D('',#26129,#15009,#15010);
#13146=AXIS2_PLACEMENT_3D('',#26130,#15011,#15012);
#13147=AXIS2_PLACEMENT_3D('',#26146,#15014,#15015);
#13148=AXIS2_PLACEMENT_3D('',#26156,#15016,#15017);
#13149=AXIS2_PLACEMENT_3D('',#26181,#15019,#15020);
#13150=AXIS2_PLACEMENT_3D('',#26206,#15022,#15023);
#13151=AXIS2_PLACEMENT_3D('',#26231,#15025,#15026);
#13152=AXIS2_PLACEMENT_3D('',#26255,#15028,#15029);
#13153=AXIS2_PLACEMENT_3D('',#26310,#15030,#15031);
#13154=AXIS2_PLACEMENT_3D('',#26312,#15032,#15033);
#13155=AXIS2_PLACEMENT_3D('',#26611,#15034,#15035);
#13156=AXIS2_PLACEMENT_3D('',#26613,#15036,#15037);
#13157=AXIS2_PLACEMENT_3D('',#26614,#15038,#15039);
#13158=AXIS2_PLACEMENT_3D('',#26671,#15040,#15041);
#13159=AXIS2_PLACEMENT_3D('',#26672,#15042,#15043);
#13160=AXIS2_PLACEMENT_3D('',#26859,#15044,#15045);
#13161=AXIS2_PLACEMENT_3D('',#26868,#15050,#15051);
#13162=AXIS2_PLACEMENT_3D('',#26874,#15055,#15056);
#13163=AXIS2_PLACEMENT_3D('',#26880,#15060,#15061);
#13164=AXIS2_PLACEMENT_3D('',#26886,#15065,#15066);
#13165=AXIS2_PLACEMENT_3D('',#26892,#15070,#15071);
#13166=AXIS2_PLACEMENT_3D('',#26895,#15074,#15075);
#13167=AXIS2_PLACEMENT_3D('',#26896,#15076,#15077);
#13168=AXIS2_PLACEMENT_3D('',#26898,#15078,#15079);
#13169=AXIS2_PLACEMENT_3D('',#26899,#15080,#15081);
#13170=AXIS2_PLACEMENT_3D('',#26901,#15083,#15084);
#13171=AXIS2_PLACEMENT_3D('',#26902,#15085,#15086);
#13172=AXIS2_PLACEMENT_3D('',#26903,#15087,#15088);
#13173=AXIS2_PLACEMENT_3D('',#26905,#15089,#15090);
#13174=AXIS2_PLACEMENT_3D('',#26907,#15092,#15093);
#13175=AXIS2_PLACEMENT_3D('',#26908,#15094,#15095);
#13176=AXIS2_PLACEMENT_3D('',#26909,#15096,#15097);
#13177=AXIS2_PLACEMENT_3D('',#26925,#15099,#15100);
#13178=AXIS2_PLACEMENT_3D('',#26933,#15101,#15102);
#13179=AXIS2_PLACEMENT_3D('',#26981,#15104,#15105);
#13180=AXIS2_PLACEMENT_3D('',#27029,#15107,#15108);
#13181=AXIS2_PLACEMENT_3D('',#27080,#15110,#15111);
#13182=AXIS2_PLACEMENT_3D('',#27131,#15113,#15114);
#13183=AXIS2_PLACEMENT_3D('',#27179,#15116,#15117);
#13184=AXIS2_PLACEMENT_3D('',#27227,#15119,#15120);
#13185=AXIS2_PLACEMENT_3D('',#27281,#15122,#15123);
#13186=AXIS2_PLACEMENT_3D('',#27329,#15125,#15126);
#13187=AXIS2_PLACEMENT_3D('',#27377,#15128,#15129);
#13188=AXIS2_PLACEMENT_3D('',#27431,#15131,#15132);
#13189=AXIS2_PLACEMENT_3D('',#27479,#15134,#15135);
#13190=AXIS2_PLACEMENT_3D('',#27527,#15137,#15138);
#13191=AXIS2_PLACEMENT_3D('',#27575,#15140,#15141);
#13192=AXIS2_PLACEMENT_3D('',#27629,#15143,#15144);
#13193=AXIS2_PLACEMENT_3D('',#27677,#15146,#15147);
#13194=AXIS2_PLACEMENT_3D('',#27725,#15149,#15150);
#13195=AXIS2_PLACEMENT_3D('',#27779,#15152,#15153);
#13196=AXIS2_PLACEMENT_3D('',#27827,#15155,#15156);
#13197=AXIS2_PLACEMENT_3D('',#27875,#15158,#15159);
#13198=AXIS2_PLACEMENT_3D('',#27926,#15161,#15162);
#13199=AXIS2_PLACEMENT_3D('',#27974,#15164,#15165);
#13200=AXIS2_PLACEMENT_3D('',#28022,#15167,#15168);
#13201=AXIS2_PLACEMENT_3D('',#28070,#15170,#15171);
#13202=AXIS2_PLACEMENT_3D('',#28079,#15173,#15174);
#13203=AXIS2_PLACEMENT_3D('',#28080,#15175,#15176);
#13204=AXIS2_PLACEMENT_3D('',#28095,#15178,#15179);
#13205=AXIS2_PLACEMENT_3D('',#28105,#15180,#15181);
#13206=AXIS2_PLACEMENT_3D('',#28129,#15183,#15184);
#13207=AXIS2_PLACEMENT_3D('',#28153,#15186,#15187);
#13208=AXIS2_PLACEMENT_3D('',#28178,#15189,#15190);
#13209=AXIS2_PLACEMENT_3D('',#28203,#15192,#15193);
#13210=AXIS2_PLACEMENT_3D('',#28227,#15195,#15196);
#13211=AXIS2_PLACEMENT_3D('',#28252,#15198,#15199);
#13212=AXIS2_PLACEMENT_3D('',#28277,#15201,#15202);
#13213=AXIS2_PLACEMENT_3D('',#28301,#15204,#15205);
#13214=AXIS2_PLACEMENT_3D('',#28326,#15207,#15208);
#13215=AXIS2_PLACEMENT_3D('',#28351,#15210,#15211);
#13216=AXIS2_PLACEMENT_3D('',#28375,#15213,#15214);
#13217=AXIS2_PLACEMENT_3D('',#28399,#15216,#15217);
#13218=AXIS2_PLACEMENT_3D('',#28424,#15219,#15220);
#13219=AXIS2_PLACEMENT_3D('',#28449,#15222,#15223);
#13220=AXIS2_PLACEMENT_3D('',#28473,#15225,#15226);
#13221=AXIS2_PLACEMENT_3D('',#28498,#15228,#15229);
#13222=AXIS2_PLACEMENT_3D('',#28523,#15231,#15232);
#13223=AXIS2_PLACEMENT_3D('',#28547,#15234,#15235);
#13224=AXIS2_PLACEMENT_3D('',#28572,#15237,#15238);
#13225=AXIS2_PLACEMENT_3D('',#28596,#15240,#15241);
#13226=AXIS2_PLACEMENT_3D('',#28621,#15243,#15244);
#13227=AXIS2_PLACEMENT_3D('',#29398,#15246,#15247);
#13228=AXIS2_PLACEMENT_3D('',#29400,#15248,#15249);
#13229=AXIS2_PLACEMENT_3D('',#29401,#15250,#15251);
#13230=AXIS2_PLACEMENT_3D('',#29461,#15252,#15253);
#13231=AXIS2_PLACEMENT_3D('',#29462,#15254,#15255);
#13232=AXIS2_PLACEMENT_3D('',#30153,#15256,#15257);
#13233=AXIS2_PLACEMENT_3D('',#30157,#15259,#15260);
#13234=AXIS2_PLACEMENT_3D('',#30158,#15261,#15262);
#13235=AXIS2_PLACEMENT_3D('',#30167,#15267,#15268);
#13236=AXIS2_PLACEMENT_3D('',#30173,#15272,#15273);
#13237=AXIS2_PLACEMENT_3D('',#30179,#15277,#15278);
#13238=AXIS2_PLACEMENT_3D('',#30185,#15282,#15283);
#13239=AXIS2_PLACEMENT_3D('',#30191,#15287,#15288);
#13240=AXIS2_PLACEMENT_3D('',#30194,#15291,#15292);
#13241=AXIS2_PLACEMENT_3D('',#30195,#15293,#15294);
#13242=AXIS2_PLACEMENT_3D('',#30204,#15299,#15300);
#13243=AXIS2_PLACEMENT_3D('',#30206,#15301,#15302);
#13244=AXIS2_PLACEMENT_3D('',#30208,#15304,#15305);
#13245=AXIS2_PLACEMENT_3D('',#30212,#15308,#15309);
#13246=AXIS2_PLACEMENT_3D('',#30213,#15310,#15311);
#13247=AXIS2_PLACEMENT_3D('',#30214,#15312,#15313);
#13248=AXIS2_PLACEMENT_3D('',#30223,#15318,#15319);
#13249=AXIS2_PLACEMENT_3D('',#30225,#15320,#15321);
#13250=AXIS2_PLACEMENT_3D('',#30227,#15323,#15324);
#13251=AXIS2_PLACEMENT_3D('',#30231,#15327,#15328);
#13252=AXIS2_PLACEMENT_3D('',#30232,#15329,#15330);
#13253=AXIS2_PLACEMENT_3D('',#30233,#15331,#15332);
#13254=AXIS2_PLACEMENT_3D('',#30242,#15337,#15338);
#13255=AXIS2_PLACEMENT_3D('',#30244,#15339,#15340);
#13256=AXIS2_PLACEMENT_3D('',#30246,#15342,#15343);
#13257=AXIS2_PLACEMENT_3D('',#30250,#15346,#15347);
#13258=AXIS2_PLACEMENT_3D('',#30251,#15348,#15349);
#13259=AXIS2_PLACEMENT_3D('',#30252,#15350,#15351);
#13260=AXIS2_PLACEMENT_3D('',#30261,#15356,#15357);
#13261=AXIS2_PLACEMENT_3D('',#30263,#15358,#15359);
#13262=AXIS2_PLACEMENT_3D('',#30265,#15361,#15362);
#13263=AXIS2_PLACEMENT_3D('',#30269,#15365,#15366);
#13264=AXIS2_PLACEMENT_3D('',#30270,#15367,#15368);
#13265=AXIS2_PLACEMENT_3D('',#30271,#15369,#15370);
#13266=AXIS2_PLACEMENT_3D('',#30280,#15375,#15376);
#13267=AXIS2_PLACEMENT_3D('',#30282,#15377,#15378);
#13268=AXIS2_PLACEMENT_3D('',#30284,#15380,#15381);
#13269=AXIS2_PLACEMENT_3D('',#30288,#15384,#15385);
#13270=AXIS2_PLACEMENT_3D('',#30289,#15386,#15387);
#13271=AXIS2_PLACEMENT_3D('',#30290,#15388,#15389);
#13272=AXIS2_PLACEMENT_3D('',#30299,#15394,#15395);
#13273=AXIS2_PLACEMENT_3D('',#30301,#15396,#15397);
#13274=AXIS2_PLACEMENT_3D('',#30303,#15399,#15400);
#13275=AXIS2_PLACEMENT_3D('',#30307,#15403,#15404);
#13276=AXIS2_PLACEMENT_3D('',#30308,#15405,#15406);
#13277=AXIS2_PLACEMENT_3D('',#30309,#15407,#15408);
#13278=AXIS2_PLACEMENT_3D('',#30318,#15413,#15414);
#13279=AXIS2_PLACEMENT_3D('',#30320,#15415,#15416);
#13280=AXIS2_PLACEMENT_3D('',#30322,#15418,#15419);
#13281=AXIS2_PLACEMENT_3D('',#30326,#15422,#15423);
#13282=AXIS2_PLACEMENT_3D('',#30327,#15424,#15425);
#13283=AXIS2_PLACEMENT_3D('',#30328,#15426,#15427);
#13284=AXIS2_PLACEMENT_3D('',#30337,#15432,#15433);
#13285=AXIS2_PLACEMENT_3D('',#30339,#15434,#15435);
#13286=AXIS2_PLACEMENT_3D('',#30341,#15437,#15438);
#13287=AXIS2_PLACEMENT_3D('',#30345,#15441,#15442);
#13288=AXIS2_PLACEMENT_3D('',#30346,#15443,#15444);
#13289=AXIS2_PLACEMENT_3D('',#30347,#15445,#15446);
#13290=AXIS2_PLACEMENT_3D('',#30356,#15451,#15452);
#13291=AXIS2_PLACEMENT_3D('',#30358,#15453,#15454);
#13292=AXIS2_PLACEMENT_3D('',#30361,#15456,#15457);
#13293=AXIS2_PLACEMENT_3D('',#30362,#15458,#15459);
#13294=AXIS2_PLACEMENT_3D('',#30366,#15462,#15463);
#13295=AXIS2_PLACEMENT_3D('',#30368,#15464,#15465);
#13296=AXIS2_PLACEMENT_3D('',#30369,#15466,#15467);
#13297=AXIS2_PLACEMENT_3D('',#30370,#15468,#15469);
#13298=AXIS2_PLACEMENT_3D('',#30379,#15474,#15475);
#13299=AXIS2_PLACEMENT_3D('',#30381,#15476,#15477);
#13300=AXIS2_PLACEMENT_3D('',#30383,#15479,#15480);
#13301=AXIS2_PLACEMENT_3D('',#30387,#15483,#15484);
#13302=AXIS2_PLACEMENT_3D('',#30388,#15485,#15486);
#13303=AXIS2_PLACEMENT_3D('',#30389,#15487,#15488);
#13304=AXIS2_PLACEMENT_3D('',#30398,#15493,#15494);
#13305=AXIS2_PLACEMENT_3D('',#30400,#15495,#15496);
#13306=AXIS2_PLACEMENT_3D('',#30402,#15498,#15499);
#13307=AXIS2_PLACEMENT_3D('',#30406,#15502,#15503);
#13308=AXIS2_PLACEMENT_3D('',#30407,#15504,#15505);
#13309=AXIS2_PLACEMENT_3D('',#30408,#15506,#15507);
#13310=AXIS2_PLACEMENT_3D('',#30417,#15512,#15513);
#13311=AXIS2_PLACEMENT_3D('',#30419,#15514,#15515);
#13312=AXIS2_PLACEMENT_3D('',#30421,#15517,#15518);
#13313=AXIS2_PLACEMENT_3D('',#30425,#15521,#15522);
#13314=AXIS2_PLACEMENT_3D('',#30426,#15523,#15524);
#13315=AXIS2_PLACEMENT_3D('',#30427,#15525,#15526);
#13316=AXIS2_PLACEMENT_3D('',#30436,#15531,#15532);
#13317=AXIS2_PLACEMENT_3D('',#30438,#15533,#15534);
#13318=AXIS2_PLACEMENT_3D('',#30440,#15536,#15537);
#13319=AXIS2_PLACEMENT_3D('',#30444,#15540,#15541);
#13320=AXIS2_PLACEMENT_3D('',#30445,#15542,#15543);
#13321=AXIS2_PLACEMENT_3D('',#30446,#15544,#15545);
#13322=AXIS2_PLACEMENT_3D('',#30455,#15550,#15551);
#13323=AXIS2_PLACEMENT_3D('',#30457,#15552,#15553);
#13324=AXIS2_PLACEMENT_3D('',#30459,#15555,#15556);
#13325=AXIS2_PLACEMENT_3D('',#30463,#15559,#15560);
#13326=AXIS2_PLACEMENT_3D('',#30464,#15561,#15562);
#13327=AXIS2_PLACEMENT_3D('',#30465,#15563,#15564);
#13328=AXIS2_PLACEMENT_3D('',#30474,#15569,#15570);
#13329=AXIS2_PLACEMENT_3D('',#30476,#15571,#15572);
#13330=AXIS2_PLACEMENT_3D('',#30478,#15574,#15575);
#13331=AXIS2_PLACEMENT_3D('',#30482,#15578,#15579);
#13332=AXIS2_PLACEMENT_3D('',#30483,#15580,#15581);
#13333=AXIS2_PLACEMENT_3D('',#30484,#15582,#15583);
#13334=AXIS2_PLACEMENT_3D('',#30493,#15588,#15589);
#13335=AXIS2_PLACEMENT_3D('',#30495,#15590,#15591);
#13336=AXIS2_PLACEMENT_3D('',#30497,#15593,#15594);
#13337=AXIS2_PLACEMENT_3D('',#30501,#15597,#15598);
#13338=AXIS2_PLACEMENT_3D('',#30502,#15599,#15600);
#13339=AXIS2_PLACEMENT_3D('',#30503,#15601,#15602);
#13340=AXIS2_PLACEMENT_3D('',#30512,#15607,#15608);
#13341=AXIS2_PLACEMENT_3D('',#30514,#15609,#15610);
#13342=AXIS2_PLACEMENT_3D('',#30516,#15612,#15613);
#13343=AXIS2_PLACEMENT_3D('',#30520,#15616,#15617);
#13344=AXIS2_PLACEMENT_3D('',#30521,#15618,#15619);
#13345=AXIS2_PLACEMENT_3D('',#30522,#15620,#15621);
#13346=AXIS2_PLACEMENT_3D('',#30531,#15626,#15627);
#13347=AXIS2_PLACEMENT_3D('',#30533,#15628,#15629);
#13348=AXIS2_PLACEMENT_3D('',#30535,#15631,#15632);
#13349=AXIS2_PLACEMENT_3D('',#30539,#15635,#15636);
#13350=AXIS2_PLACEMENT_3D('',#30540,#15637,#15638);
#13351=AXIS2_PLACEMENT_3D('',#30541,#15639,#15640);
#13352=AXIS2_PLACEMENT_3D('',#30550,#15645,#15646);
#13353=AXIS2_PLACEMENT_3D('',#30552,#15647,#15648);
#13354=AXIS2_PLACEMENT_3D('',#30554,#15650,#15651);
#13355=AXIS2_PLACEMENT_3D('',#30558,#15654,#15655);
#13356=AXIS2_PLACEMENT_3D('',#30559,#15656,#15657);
#13357=AXIS2_PLACEMENT_3D('',#30560,#15658,#15659);
#13358=AXIS2_PLACEMENT_3D('',#30569,#15664,#15665);
#13359=AXIS2_PLACEMENT_3D('',#30571,#15666,#15667);
#13360=AXIS2_PLACEMENT_3D('',#30573,#15669,#15670);
#13361=AXIS2_PLACEMENT_3D('',#30577,#15673,#15674);
#13362=AXIS2_PLACEMENT_3D('',#30578,#15675,#15676);
#13363=AXIS2_PLACEMENT_3D('',#30579,#15677,#15678);
#13364=AXIS2_PLACEMENT_3D('',#30588,#15683,#15684);
#13365=AXIS2_PLACEMENT_3D('',#30590,#15685,#15686);
#13366=AXIS2_PLACEMENT_3D('',#30592,#15688,#15689);
#13367=AXIS2_PLACEMENT_3D('',#30596,#15692,#15693);
#13368=AXIS2_PLACEMENT_3D('',#30597,#15694,#15695);
#13369=AXIS2_PLACEMENT_3D('',#30598,#15696,#15697);
#13370=AXIS2_PLACEMENT_3D('',#30607,#15702,#15703);
#13371=AXIS2_PLACEMENT_3D('',#30609,#15704,#15705);
#13372=AXIS2_PLACEMENT_3D('',#30611,#15707,#15708);
#13373=AXIS2_PLACEMENT_3D('',#30615,#15711,#15712);
#13374=AXIS2_PLACEMENT_3D('',#30616,#15713,#15714);
#13375=AXIS2_PLACEMENT_3D('',#30617,#15715,#15716);
#13376=AXIS2_PLACEMENT_3D('',#30626,#15721,#15722);
#13377=AXIS2_PLACEMENT_3D('',#30628,#15723,#15724);
#13378=AXIS2_PLACEMENT_3D('',#30630,#15726,#15727);
#13379=AXIS2_PLACEMENT_3D('',#30634,#15730,#15731);
#13380=AXIS2_PLACEMENT_3D('',#30635,#15732,#15733);
#13381=AXIS2_PLACEMENT_3D('',#30636,#15734,#15735);
#13382=AXIS2_PLACEMENT_3D('',#30645,#15740,#15741);
#13383=AXIS2_PLACEMENT_3D('',#30647,#15742,#15743);
#13384=AXIS2_PLACEMENT_3D('',#30649,#15745,#15746);
#13385=AXIS2_PLACEMENT_3D('',#30653,#15749,#15750);
#13386=AXIS2_PLACEMENT_3D('',#30654,#15751,#15752);
#13387=AXIS2_PLACEMENT_3D('',#30655,#15753,#15754);
#13388=AXIS2_PLACEMENT_3D('',#30664,#15759,#15760);
#13389=AXIS2_PLACEMENT_3D('',#30666,#15761,#15762);
#13390=AXIS2_PLACEMENT_3D('',#30668,#15764,#15765);
#13391=AXIS2_PLACEMENT_3D('',#30672,#15768,#15769);
#13392=AXIS2_PLACEMENT_3D('',#30673,#15770,#15771);
#13393=AXIS2_PLACEMENT_3D('',#30674,#15772,#15773);
#13394=AXIS2_PLACEMENT_3D('',#30683,#15778,#15779);
#13395=AXIS2_PLACEMENT_3D('',#30685,#15780,#15781);
#13396=AXIS2_PLACEMENT_3D('',#30687,#15783,#15784);
#13397=AXIS2_PLACEMENT_3D('',#30691,#15787,#15788);
#13398=AXIS2_PLACEMENT_3D('',#30692,#15789,#15790);
#13399=AXIS2_PLACEMENT_3D('',#30693,#15791,#15792);
#13400=AXIS2_PLACEMENT_3D('',#30696,#15793,#15794);
#13401=AXIS2_PLACEMENT_3D('',#30700,#15797,#15798);
#13402=AXIS2_PLACEMENT_3D('',#30706,#15802,#15803);
#13403=AXIS2_PLACEMENT_3D('',#30710,#15806,#15807);
#13404=AXIS2_PLACEMENT_3D('',#30711,#15808,#15809);
#13405=AXIS2_PLACEMENT_3D('',#30712,#15810,#15811);
#13406=AXIS2_PLACEMENT_3D('',#30721,#15816,#15817);
#13407=AXIS2_PLACEMENT_3D('',#30723,#15818,#15819);
#13408=AXIS2_PLACEMENT_3D('',#30725,#15821,#15822);
#13409=AXIS2_PLACEMENT_3D('',#30729,#15825,#15826);
#13410=AXIS2_PLACEMENT_3D('',#30730,#15827,#15828);
#13411=AXIS2_PLACEMENT_3D('',#30731,#15829,#15830);
#13412=AXIS2_PLACEMENT_3D('',#30740,#15835,#15836);
#13413=AXIS2_PLACEMENT_3D('',#30742,#15837,#15838);
#13414=AXIS2_PLACEMENT_3D('',#30744,#15840,#15841);
#13415=AXIS2_PLACEMENT_3D('',#30748,#15844,#15845);
#13416=AXIS2_PLACEMENT_3D('',#30749,#15846,#15847);
#13417=AXIS2_PLACEMENT_3D('',#30750,#15848,#15849);
#13418=AXIS2_PLACEMENT_3D('',#30759,#15854,#15855);
#13419=AXIS2_PLACEMENT_3D('',#30761,#15856,#15857);
#13420=AXIS2_PLACEMENT_3D('',#30763,#15859,#15860);
#13421=AXIS2_PLACEMENT_3D('',#30767,#15863,#15864);
#13422=AXIS2_PLACEMENT_3D('',#30768,#15865,#15866);
#13423=AXIS2_PLACEMENT_3D('',#30769,#15867,#15868);
#13424=AXIS2_PLACEMENT_3D('',#30778,#15873,#15874);
#13425=AXIS2_PLACEMENT_3D('',#30780,#15875,#15876);
#13426=AXIS2_PLACEMENT_3D('',#30782,#15878,#15879);
#13427=AXIS2_PLACEMENT_3D('',#30786,#15882,#15883);
#13428=AXIS2_PLACEMENT_3D('',#30787,#15884,#15885);
#13429=AXIS2_PLACEMENT_3D('',#30788,#15886,#15887);
#13430=AXIS2_PLACEMENT_3D('',#30797,#15892,#15893);
#13431=AXIS2_PLACEMENT_3D('',#30799,#15894,#15895);
#13432=AXIS2_PLACEMENT_3D('',#30801,#15897,#15898);
#13433=AXIS2_PLACEMENT_3D('',#30805,#15901,#15902);
#13434=AXIS2_PLACEMENT_3D('',#30806,#15903,#15904);
#13435=AXIS2_PLACEMENT_3D('',#30807,#15905,#15906);
#13436=AXIS2_PLACEMENT_3D('',#30816,#15911,#15912);
#13437=AXIS2_PLACEMENT_3D('',#30818,#15913,#15914);
#13438=AXIS2_PLACEMENT_3D('',#30820,#15916,#15917);
#13439=AXIS2_PLACEMENT_3D('',#30824,#15920,#15921);
#13440=AXIS2_PLACEMENT_3D('',#30825,#15922,#15923);
#13441=AXIS2_PLACEMENT_3D('',#30826,#15924,#15925);
#13442=AXIS2_PLACEMENT_3D('',#30835,#15930,#15931);
#13443=AXIS2_PLACEMENT_3D('',#30837,#15932,#15933);
#13444=AXIS2_PLACEMENT_3D('',#30839,#15935,#15936);
#13445=AXIS2_PLACEMENT_3D('',#30843,#15939,#15940);
#13446=AXIS2_PLACEMENT_3D('',#30844,#15941,#15942);
#13447=AXIS2_PLACEMENT_3D('',#30845,#15943,#15944);
#13448=AXIS2_PLACEMENT_3D('',#30854,#15949,#15950);
#13449=AXIS2_PLACEMENT_3D('',#30856,#15951,#15952);
#13450=AXIS2_PLACEMENT_3D('',#30858,#15954,#15955);
#13451=AXIS2_PLACEMENT_3D('',#30862,#15958,#15959);
#13452=AXIS2_PLACEMENT_3D('',#30863,#15960,#15961);
#13453=AXIS2_PLACEMENT_3D('',#30864,#15962,#15963);
#13454=AXIS2_PLACEMENT_3D('',#30873,#15968,#15969);
#13455=AXIS2_PLACEMENT_3D('',#30875,#15970,#15971);
#13456=AXIS2_PLACEMENT_3D('',#30877,#15973,#15974);
#13457=AXIS2_PLACEMENT_3D('',#30881,#15977,#15978);
#13458=AXIS2_PLACEMENT_3D('',#30882,#15979,#15980);
#13459=AXIS2_PLACEMENT_3D('',#30883,#15981,#15982);
#13460=AXIS2_PLACEMENT_3D('',#30885,#15983,#15984);
#13461=AXIS2_PLACEMENT_3D('',#30887,#15985,#15986);
#13462=AXIS2_PLACEMENT_3D('',#30888,#15987,#15988);
#13463=AXIS2_PLACEMENT_3D('',#30889,#15989,#15990);
#13464=AXIS2_PLACEMENT_3D('',#30892,#15992,#15993);
#13465=AXIS2_PLACEMENT_3D('',#30893,#15994,#15995);
#13466=AXIS2_PLACEMENT_3D('',#30895,#15996,#15997);
#13467=AXIS2_PLACEMENT_3D('',#30896,#15998,#15999);
#13468=AXIS2_PLACEMENT_3D('',#30898,#16000,#16001);
#13469=AXIS2_PLACEMENT_3D('',#30899,#16002,#16003);
#13470=AXIS2_PLACEMENT_3D('',#30901,#16005,#16006);
#13471=AXIS2_PLACEMENT_3D('',#30902,#16007,#16008);
#13472=AXIS2_PLACEMENT_3D('',#30903,#16009,#16010);
#13473=AXIS2_PLACEMENT_3D('',#30904,#16011,#16012);
#13474=AXIS2_PLACEMENT_3D('',#30906,#16013,#16014);
#13475=AXIS2_PLACEMENT_3D('',#30908,#16016,#16017);
#13476=AXIS2_PLACEMENT_3D('',#30909,#16018,#16019);
#13477=AXIS2_PLACEMENT_3D('',#30910,#16020,#16021);
#13478=AXIS2_PLACEMENT_3D('',#30911,#16022,#16023);
#13479=AXIS2_PLACEMENT_3D('',#30912,#16024,#16025);
#13480=AXIS2_PLACEMENT_3D('',#30913,#16026,#16027);
#13481=AXIS2_PLACEMENT_3D('',#30914,#16028,#16029);
#13482=AXIS2_PLACEMENT_3D('',#30915,#16030,#16031);
#13483=AXIS2_PLACEMENT_3D('',#30916,#16032,#16033);
#13484=AXIS2_PLACEMENT_3D('',#30917,#16034,#16035);
#13485=AXIS2_PLACEMENT_3D('',#30918,#16036,#16037);
#13486=AXIS2_PLACEMENT_3D('',#30919,#16038,#16039);
#13487=AXIS2_PLACEMENT_3D('',#30920,#16040,#16041);
#13488=AXIS2_PLACEMENT_3D('',#30921,#16042,#16043);
#13489=AXIS2_PLACEMENT_3D('',#30922,#16044,#16045);
#13490=AXIS2_PLACEMENT_3D('',#30923,#16046,#16047);
#13491=AXIS2_PLACEMENT_3D('',#30924,#16048,#16049);
#13492=AXIS2_PLACEMENT_3D('',#30926,#16051,#16052);
#13493=AXIS2_PLACEMENT_3D('',#30927,#16053,#16054);
#13494=AXIS2_PLACEMENT_3D('',#30928,#16055,#16056);
#13495=AXIS2_PLACEMENT_3D('',#30929,#16057,#16058);
#13496=AXIS2_PLACEMENT_3D('',#30930,#16059,#16060);
#13497=AXIS2_PLACEMENT_3D('',#30931,#16061,#16062);
#13498=AXIS2_PLACEMENT_3D('',#30932,#16063,#16064);
#13499=AXIS2_PLACEMENT_3D('',#30933,#16065,#16066);
#13500=AXIS2_PLACEMENT_3D('',#30934,#16067,#16068);
#13501=AXIS2_PLACEMENT_3D('',#30935,#16069,#16070);
#13502=AXIS2_PLACEMENT_3D('',#30936,#16071,#16072);
#13503=AXIS2_PLACEMENT_3D('',#30937,#16073,#16074);
#13504=AXIS2_PLACEMENT_3D('',#30938,#16075,#16076);
#13505=AXIS2_PLACEMENT_3D('',#30939,#16077,#16078);
#13506=AXIS2_PLACEMENT_3D('',#30940,#16079,#16080);
#13507=AXIS2_PLACEMENT_3D('',#30941,#16081,#16082);
#13508=AXIS2_PLACEMENT_3D('',#30942,#16083,#16084);
#13509=AXIS2_PLACEMENT_3D('',#30943,#16085,#16086);
#13510=AXIS2_PLACEMENT_3D('',#30944,#16087,#16088);
#13511=AXIS2_PLACEMENT_3D('',#30945,#16089,#16090);
#13512=AXIS2_PLACEMENT_3D('',#30946,#16091,#16092);
#13513=AXIS2_PLACEMENT_3D('',#30948,#16093,#16094);
#13514=AXIS2_PLACEMENT_3D('',#30950,#16096,#16097);
#13515=AXIS2_PLACEMENT_3D('',#30951,#16098,#16099);
#13516=AXIS2_PLACEMENT_3D('',#30952,#16100,#16101);
#13517=AXIS2_PLACEMENT_3D('',#30954,#16102,#16103);
#13518=AXIS2_PLACEMENT_3D('',#30958,#16105,#16106);
#13519=AXIS2_PLACEMENT_3D('',#30959,#16107,#16108);
#13520=AXIS2_PLACEMENT_3D('',#30960,#16109,#16110);
#13521=AXIS2_PLACEMENT_3D('',#30962,#16111,#16112);
#13522=AXIS2_PLACEMENT_3D('',#30963,#16113,#16114);
#13523=AXIS2_PLACEMENT_3D('',#30966,#16116,#16117);
#13524=AXIS2_PLACEMENT_3D('',#30967,#16118,#16119);
#13525=AXIS2_PLACEMENT_3D('',#30969,#16120,#16121);
#13526=AXIS2_PLACEMENT_3D('',#30973,#16123,#16124);
#13527=AXIS2_PLACEMENT_3D('',#30974,#16125,#16126);
#13528=AXIS2_PLACEMENT_3D('',#30975,#16127,#16128);
#13529=AXIS2_PLACEMENT_3D('',#30978,#16129,#16130);
#13530=AXIS2_PLACEMENT_3D('',#30979,#16131,#16132);
#13531=AXIS2_PLACEMENT_3D('',#30981,#16134,#16135);
#13532=AXIS2_PLACEMENT_3D('',#30983,#16136,#16137);
#13533=AXIS2_PLACEMENT_3D('',#30984,#16138,#16139);
#13534=AXIS2_PLACEMENT_3D('',#30986,#16141,#16142);
#13535=AXIS2_PLACEMENT_3D('',#30988,#16144,#16145);
#13536=AXIS2_PLACEMENT_3D('',#30989,#16146,#16147);
#13537=AXIS2_PLACEMENT_3D('',#31006,#16149,#16150);
#13538=AXIS2_PLACEMENT_3D('',#31023,#16152,#16153);
#13539=AXIS2_PLACEMENT_3D('',#31040,#16155,#16156);
#13540=AXIS2_PLACEMENT_3D('',#31057,#16158,#16159);
#13541=AXIS2_PLACEMENT_3D('',#31074,#16161,#16162);
#13542=AXIS2_PLACEMENT_3D('',#31151,#16164,#16165);
#13543=AXIS2_PLACEMENT_3D('',#31279,#16168,#16169);
#13544=AXIS2_PLACEMENT_3D('',#31287,#16172,#16173);
#13545=AXIS2_PLACEMENT_3D('',#31420,#16176,#16177);
#13546=AXIS2_PLACEMENT_3D('',#31428,#16180,#16181);
#13547=AXIS2_PLACEMENT_3D('',#31496,#16184,#16185);
#13548=AXIS2_PLACEMENT_3D('',#31504,#16188,#16189);
#13549=AXIS2_PLACEMENT_3D('',#31508,#16190,#16191);
#13550=AXIS2_PLACEMENT_3D('',#31512,#16192,#16193);
#13551=AXIS2_PLACEMENT_3D('',#31516,#16194,#16195);
#13552=AXIS2_PLACEMENT_3D('',#31518,#16196,#16197);
#13553=AXIS2_PLACEMENT_3D('',#31533,#16199,#16200);
#13554=AXIS2_PLACEMENT_3D('',#31534,#16201,#16202);
#13555=AXIS2_PLACEMENT_3D('',#31535,#16203,#16204);
#13556=AXIS2_PLACEMENT_3D('',#31536,#16205,#16206);
#13557=AXIS2_PLACEMENT_3D('',#31537,#16207,#16208);
#13558=AXIS2_PLACEMENT_3D('',#31538,#16209,#16210);
#13559=AXIS2_PLACEMENT_3D('',#31539,#16211,#16212);
#13560=AXIS2_PLACEMENT_3D('',#31540,#16213,#16214);
#13561=AXIS2_PLACEMENT_3D('',#31541,#16215,#16216);
#13562=AXIS2_PLACEMENT_3D('',#31542,#16217,#16218);
#13563=AXIS2_PLACEMENT_3D('',#31543,#16219,#16220);
#13564=AXIS2_PLACEMENT_3D('',#31544,#16221,#16222);
#13565=AXIS2_PLACEMENT_3D('',#31545,#16223,#16224);
#13566=AXIS2_PLACEMENT_3D('',#31547,#16225,#16226);
#13567=AXIS2_PLACEMENT_3D('',#31549,#16228,#16229);
#13568=AXIS2_PLACEMENT_3D('',#31551,#16230,#16231);
#13569=AXIS2_PLACEMENT_3D('',#31552,#16232,#16233);
#13570=AXIS2_PLACEMENT_3D('',#31554,#16234,#16235);
#13571=AXIS2_PLACEMENT_3D('',#31556,#16237,#16238);
#13572=AXIS2_PLACEMENT_3D('',#31559,#16240,#16241);
#13573=AXIS2_PLACEMENT_3D('',#31560,#16242,#16243);
#13574=AXIS2_PLACEMENT_3D('',#31563,#16245,#16246);
#13575=AXIS2_PLACEMENT_3D('',#31564,#16247,#16248);
#13576=AXIS2_PLACEMENT_3D('',#31567,#16250,#16251);
#13577=AXIS2_PLACEMENT_3D('',#31568,#16252,#16253);
#13578=AXIS2_PLACEMENT_3D('',#31571,#16255,#16256);
#13579=AXIS2_PLACEMENT_3D('',#31572,#16257,#16258);
#13580=AXIS2_PLACEMENT_3D('',#31573,#16259,#16260);
#13581=AXIS2_PLACEMENT_3D('',#31574,#16261,#16262);
#13582=AXIS2_PLACEMENT_3D('',#31575,#16263,#16264);
#13583=AXIS2_PLACEMENT_3D('',#31576,#16265,#16266);
#13584=AXIS2_PLACEMENT_3D('',#31577,#16267,#16268);
#13585=AXIS2_PLACEMENT_3D('',#31578,#16269,#16270);
#13586=AXIS2_PLACEMENT_3D('',#31579,#16271,#16272);
#13587=AXIS2_PLACEMENT_3D('',#31580,#16273,#16274);
#13588=AXIS2_PLACEMENT_3D('',#31581,#16275,#16276);
#13589=AXIS2_PLACEMENT_3D('',#31582,#16277,#16278);
#13590=AXIS2_PLACEMENT_3D('',#31583,#16279,#16280);
#13591=AXIS2_PLACEMENT_3D('',#31584,#16281,#16282);
#13592=AXIS2_PLACEMENT_3D('',#31585,#16283,#16284);
#13593=AXIS2_PLACEMENT_3D('',#31586,#16285,#16286);
#13594=AXIS2_PLACEMENT_3D('',#31587,#16287,#16288);
#13595=AXIS2_PLACEMENT_3D('',#31588,#16289,#16290);
#13596=AXIS2_PLACEMENT_3D('',#31589,#16291,#16292);
#13597=AXIS2_PLACEMENT_3D('',#31590,#16293,#16294);
#13598=AXIS2_PLACEMENT_3D('',#31591,#16295,#16296);
#13599=AXIS2_PLACEMENT_3D('',#31592,#16297,#16298);
#13600=AXIS2_PLACEMENT_3D('',#31593,#16299,#16300);
#13601=AXIS2_PLACEMENT_3D('',#31594,#16301,#16302);
#13602=AXIS2_PLACEMENT_3D('',#31595,#16303,#16304);
#13603=AXIS2_PLACEMENT_3D('',#31596,#16305,#16306);
#13604=AXIS2_PLACEMENT_3D('',#31597,#16307,#16308);
#13605=AXIS2_PLACEMENT_3D('',#31598,#16309,#16310);
#13606=AXIS2_PLACEMENT_3D('',#31599,#16311,#16312);
#13607=AXIS2_PLACEMENT_3D('',#31600,#16313,#16314);
#13608=AXIS2_PLACEMENT_3D('',#31601,#16315,#16316);
#13609=AXIS2_PLACEMENT_3D('',#31602,#16317,#16318);
#13610=AXIS2_PLACEMENT_3D('',#31603,#16319,#16320);
#13611=AXIS2_PLACEMENT_3D('',#31604,#16321,#16322);
#13612=AXIS2_PLACEMENT_3D('',#31605,#16323,#16324);
#13613=AXIS2_PLACEMENT_3D('',#31606,#16325,#16326);
#13614=AXIS2_PLACEMENT_3D('',#31607,#16327,#16328);
#13615=AXIS2_PLACEMENT_3D('',#31608,#16329,#16330);
#13616=AXIS2_PLACEMENT_3D('',#31609,#16331,#16332);
#13617=AXIS2_PLACEMENT_3D('',#31610,#16333,#16334);
#13618=AXIS2_PLACEMENT_3D('',#31611,#16335,#16336);
#13619=AXIS2_PLACEMENT_3D('',#31612,#16337,#16338);
#13620=DIRECTION('axis',(0.,0.,1.));
#13621=DIRECTION('refdir',(1.,0.,0.));
#13622=DIRECTION('axis',(0.,0.,1.));
#13623=DIRECTION('refdir',(1.,0.,0.));
#13624=DIRECTION('center_axis',(-0.923879532511287,0.,-0.382683432365089));
#13625=DIRECTION('ref_axis',(-0.382683432365089,0.,0.923879532511287));
#13626=DIRECTION('',(0.336556770590777,-0.475963149477969,-0.812519920068745));
#13627=DIRECTION('',(0.,-1.,0.));
#13628=DIRECTION('',(-0.336556770590777,-0.475963149477969,0.812519920068745));
#13629=DIRECTION('',(-0.357406744336593,0.357406744336593,0.862856209461017));
#13630=DIRECTION('',(0.,1.,0.));
#13631=DIRECTION('',(0.357406744336593,0.357406744336593,-0.862856209461017));
#13632=DIRECTION('center_axis',(-1.,0.,0.));
#13633=DIRECTION('ref_axis',(0.,0.,1.));
#13634=DIRECTION('',(0.,0.,-1.));
#13635=DIRECTION('center_axis',(-1.,0.,0.));
#13636=DIRECTION('ref_axis',(0.,-0.707106781186547,-0.707106781186548));
#13637=DIRECTION('',(0.,-1.,0.));
#13638=DIRECTION('center_axis',(-1.,0.,0.));
#13639=DIRECTION('ref_axis',(0.,0.707106781186547,-0.707106781186548));
#13640=DIRECTION('',(0.,0.,1.));
#13641=DIRECTION('center_axis',(1.,0.,0.));
#13642=DIRECTION('ref_axis',(0.,0.,1.));
#13643=DIRECTION('center_axis',(-0.707106781186548,-0.707106781186548,0.));
#13644=DIRECTION('ref_axis',(0.,0.,1.));
#13645=DIRECTION('',(0.707106781186548,-0.707106781186548,0.));
#13646=DIRECTION('',(0.,0.,-1.));
#13647=DIRECTION('',(-0.707106781186548,0.707106781186548,0.));
#13648=DIRECTION('center_axis',(-0.577350269189626,-0.577350269189626,-0.577350269189626));
#13649=DIRECTION('ref_axis',(-0.707106781186548,0.,0.707106781186547));
#13650=DIRECTION('',(-0.707106781186548,0.,0.707106781186547));
#13651=DIRECTION('',(-0.812519920068745,0.475963149477971,0.336556770590774));
#13652=DIRECTION('',(0.,0.707106781186548,-0.707106781186548));
#13653=DIRECTION('',(0.475963149477967,0.336556770590778,-0.812519920068745));
#13654=DIRECTION('',(0.812519920068746,-0.336556770590778,-0.475963149477967));
#13655=DIRECTION('center_axis',(-0.382683432365086,0.,-0.923879532511288));
#13656=DIRECTION('ref_axis',(-0.923879532511288,0.,0.382683432365086));
#13657=DIRECTION('',(0.,1.,0.));
#13658=DIRECTION('',(0.812519920068745,0.475963149477971,-0.336556770590774));
#13659=DIRECTION('',(0.862856209461019,-0.35740674433659,-0.35740674433659));
#13660=DIRECTION('',(0.,-1.,0.));
#13661=DIRECTION('',(-0.862856209461019,-0.35740674433659,0.35740674433659));
#13662=DIRECTION('center_axis',(0.,0.,-1.));
#13663=DIRECTION('ref_axis',(-1.,0.,0.));
#13664=DIRECTION('',(-1.,0.,0.));
#13665=DIRECTION('',(0.,1.,0.));
#13666=DIRECTION('',(1.,0.,0.));
#13667=DIRECTION('center_axis',(0.,0.707106781186548,-0.707106781186548));
#13668=DIRECTION('ref_axis',(-1.,0.,0.));
#13669=DIRECTION('',(0.,0.707106781186548,0.707106781186548));
#13670=DIRECTION('',(-1.,0.,0.));
#13671=DIRECTION('',(0.,-0.707106781186548,-0.707106781186548));
#13672=DIRECTION('',(0.862856209461016,0.357406744336594,0.357406744336594));
#13673=DIRECTION('center_axis',(-0.577350269189626,0.577350269189626,-0.577350269189626));
#13674=DIRECTION('ref_axis',(-0.707106781186548,0.,0.707106781186547));
#13675=DIRECTION('',(-0.707106781186548,-0.707106781186548,0.));
#13676=DIRECTION('',(-0.812519920068746,-0.336556770590778,0.475963149477967));
#13677=DIRECTION('',(-0.475963149477968,0.336556770590778,0.812519920068745));
#13678=DIRECTION('',(0.707106781186548,0.,-0.707106781186547));
#13679=DIRECTION('center_axis',(0.38268343236509,0.,-0.923879532511287));
#13680=DIRECTION('ref_axis',(-0.923879532511287,0.,-0.38268343236509));
#13681=DIRECTION('',(0.812519920068746,-0.475963149477968,0.336556770590778));
#13682=DIRECTION('',(0.,-1.,0.));
#13683=DIRECTION('',(-0.812519920068746,-0.475963149477968,-0.336556770590778));
#13684=DIRECTION('',(-0.862856209461016,0.357406744336594,-0.357406744336594));
#13685=DIRECTION('center_axis',(0.,-0.707106781186548,-0.707106781186548));
#13686=DIRECTION('ref_axis',(-1.,0.,0.));
#13687=DIRECTION('',(0.,-0.707106781186548,0.707106781186548));
#13688=DIRECTION('',(1.,0.,0.));
#13689=DIRECTION('center_axis',(0.577350269189626,-0.577350269189626,-0.577350269189626));
#13690=DIRECTION('ref_axis',(-0.707106781186548,0.,-0.707106781186548));
#13691=DIRECTION('',(-0.707106781186548,0.,-0.707106781186548));
#13692=DIRECTION('',(-0.336556770590791,0.475963149477956,-0.812519920068747));
#13693=DIRECTION('',(0.707106781186548,0.707106781186548,0.));
#13694=DIRECTION('',(0.812519920068746,0.336556770590782,0.475963149477964));
#13695=DIRECTION('',(0.475963149477967,-0.336556770590778,0.812519920068745));
#13696=DIRECTION('center_axis',(0.923879532511282,0.,-0.382683432365102));
#13697=DIRECTION('ref_axis',(-0.382683432365102,0.,-0.923879532511282));
#13698=DIRECTION('',(0.,1.,0.));
#13699=DIRECTION('',(0.336556770590791,0.475963149477956,0.812519920068747));
#13700=DIRECTION('',(0.357406744336604,-0.357406744336604,0.862856209461008));
#13701=DIRECTION('',(0.,-1.,0.));
#13702=DIRECTION('',(-0.357406744336604,-0.357406744336604,-0.862856209461008));
#13703=DIRECTION('center_axis',(1.,0.,0.));
#13704=DIRECTION('ref_axis',(0.,0.,-1.));
#13705=DIRECTION('',(0.,0.,-1.));
#13706=DIRECTION('',(0.,1.,0.));
#13707=DIRECTION('',(0.,0.,1.));
#13708=DIRECTION('center_axis',(-1.,0.,0.));
#13709=DIRECTION('ref_axis',(0.,0.,1.));
#13710=DIRECTION('center_axis',(0.707106781186548,0.707106781186548,0.));
#13711=DIRECTION('ref_axis',(0.,0.,-1.));
#13712=DIRECTION('',(-0.707106781186548,0.707106781186548,0.));
#13713=DIRECTION('',(0.,0.,-1.));
#13714=DIRECTION('',(0.707106781186548,-0.707106781186548,1.57009245868377E-14));
#13715=DIRECTION('',(-0.357406744336597,0.357406744336597,0.862856209461013));
#13716=DIRECTION('center_axis',(0.577350269189626,0.577350269189626,-0.577350269189626));
#13717=DIRECTION('ref_axis',(-0.707106781186548,0.,-0.707106781186548));
#13718=DIRECTION('',(-0.475963149477967,-0.336556770590778,-0.812519920068745));
#13719=DIRECTION('',(-0.812519920068746,0.336556770590782,-0.475963149477964));
#13720=DIRECTION('',(0.707106781186548,0.,0.707106781186548));
#13721=DIRECTION('center_axis',(0.923879532511285,0.,0.382683432365095));
#13722=DIRECTION('ref_axis',(0.382683432365095,0.,-0.923879532511285));
#13723=DIRECTION('',(-0.336556770590782,-0.475963149477969,0.812519920068743));
#13724=DIRECTION('',(0.,-1.,0.));
#13725=DIRECTION('',(0.336556770590782,-0.475963149477969,-0.812519920068743));
#13726=DIRECTION('',(0.357406744336597,0.357406744336597,-0.862856209461013));
#13727=DIRECTION('center_axis',(0.707106781186548,-0.707106781186548,0.));
#13728=DIRECTION('ref_axis',(0.,0.,-1.));
#13729=DIRECTION('',(-0.707106781186548,-0.707106781186548,-1.57009245868377E-14));
#13730=DIRECTION('',(0.,0.,1.));
#13731=DIRECTION('center_axis',(0.577350269189617,-0.57735026918963,0.57735026918963));
#13732=DIRECTION('ref_axis',(0.707106781186555,0.,-0.70710678118654));
#13733=DIRECTION('',(0.707106781186555,0.,-0.70710678118654));
#13734=DIRECTION('',(0.812519920068752,0.475963149477957,-0.336556770590777));
#13735=DIRECTION('',(0.,0.707106781186548,0.707106781186548));
#13736=DIRECTION('',(-0.475963149477975,0.336556770590777,0.812519920068742));
#13737=DIRECTION('',(-0.812519920068753,-0.336556770590785,0.47596314947795));
#13738=DIRECTION('center_axis',(0.70710678118654,0.,0.707106781186555));
#13739=DIRECTION('ref_axis',(0.707106781186555,0.,-0.70710678118654));
#13740=DIRECTION('',(-0.707106781186555,0.,0.70710678118654));
#13741=DIRECTION('',(0.,1.,0.));
#13742=DIRECTION('center_axis',(0.382683432365087,0.,0.923879532511288));
#13743=DIRECTION('ref_axis',(0.923879532511288,0.,-0.382683432365087));
#13744=DIRECTION('',(-0.812519920068752,0.475963149477957,0.336556770590777));
#13745=DIRECTION('',(-0.862856209461019,-0.357406744336591,0.357406744336591));
#13746=DIRECTION('',(0.,-1.,0.));
#13747=DIRECTION('',(0.862856209461019,-0.357406744336591,-0.357406744336591));
#13748=DIRECTION('center_axis',(0.,-0.707106781186548,0.707106781186548));
#13749=DIRECTION('ref_axis',(1.,0.,0.));
#13750=DIRECTION('',(-1.,0.,0.));
#13751=DIRECTION('',(0.862856209461006,0.357406744336607,0.357406744336607));
#13752=DIRECTION('',(0.,-0.707106781186548,-0.707106781186548));
#13753=DIRECTION('',(-1.,0.,0.));
#13754=DIRECTION('center_axis',(-0.923879532511288,0.,0.382683432365087));
#13755=DIRECTION('ref_axis',(0.382683432365087,0.,0.923879532511288));
#13756=DIRECTION('',(0.336556770590774,0.475963149477971,0.812519920068745));
#13757=DIRECTION('',(0.,1.,0.));
#13758=DIRECTION('',(-0.336556770590774,0.475963149477971,-0.812519920068745));
#13759=DIRECTION('',(-0.357406744336591,-0.357406744336591,-0.862856209461019));
#13760=DIRECTION('',(0.,-1.,0.));
#13761=DIRECTION('',(0.357406744336591,-0.357406744336591,0.862856209461019));
#13762=DIRECTION('center_axis',(-0.577350269189626,-0.577350269189626,0.577350269189626));
#13763=DIRECTION('ref_axis',(0.707106781186548,0.,0.707106781186548));
#13764=DIRECTION('',(-0.707106781186548,0.707106781186548,0.));
#13765=DIRECTION('',(-0.812519920068746,0.336556770590782,-0.475963149477964));
#13766=DIRECTION('',(-0.475963149477967,-0.336556770590779,-0.812519920068746));
#13767=DIRECTION('',(0.812519920068747,-0.475963149477952,0.336556770590795));
#13768=DIRECTION('',(0.707106781186548,0.,0.707106781186548));
#13769=DIRECTION('center_axis',(-0.707106781186548,-0.707106781186548,0.));
#13770=DIRECTION('ref_axis',(0.,0.,1.));
#13771=DIRECTION('',(0.,0.,-1.));
#13772=DIRECTION('',(-0.357406744336594,0.357406744336594,0.862856209461016));
#13773=DIRECTION('',(0.707106781186548,-0.707106781186548,0.));
#13774=DIRECTION('',(0.,0.,-1.));
#13775=DIRECTION('center_axis',(-1.,0.,0.));
#13776=DIRECTION('ref_axis',(0.,0.,1.));
#13777=DIRECTION('',(0.,0.,1.));
#13778=DIRECTION('',(0.,1.,0.));
#13779=DIRECTION('center_axis',(1.,0.,0.));
#13780=DIRECTION('ref_axis',(0.,0.,1.));
#13781=DIRECTION('center_axis',(-0.382683432365106,0.,0.92387953251128));
#13782=DIRECTION('ref_axis',(0.92387953251128,0.,0.382683432365106));
#13783=DIRECTION('',(-0.812519920068747,-0.475963149477952,-0.336556770590795));
#13784=DIRECTION('',(0.,-1.,0.));
#13785=DIRECTION('',(0.,1.,0.));
#13786=DIRECTION('',(-0.862856209461006,0.357406744336607,-0.357406744336607));
#13787=DIRECTION('center_axis',(-0.707106781186548,0.,0.707106781186548));
#13788=DIRECTION('ref_axis',(0.707106781186548,0.,0.707106781186548));
#13789=DIRECTION('',(-0.707106781186548,0.,-0.707106781186548));
#13790=DIRECTION('center_axis',(-0.577350269189626,0.577350269189626,0.577350269189626));
#13791=DIRECTION('ref_axis',(0.707106781186548,0.,0.707106781186548));
#13792=DIRECTION('',(0.,-0.707106781186548,0.707106781186548));
#13793=DIRECTION('',(0.475963149477967,-0.336556770590779,0.812519920068746));
#13794=DIRECTION('',(0.812519920068746,0.336556770590782,0.475963149477964));
#13795=DIRECTION('',(0.707106781186548,0.707106781186548,0.));
#13796=DIRECTION('center_axis',(0.,0.707106781186548,0.707106781186548));
#13797=DIRECTION('ref_axis',(1.,0.,0.));
#13798=DIRECTION('',(0.,0.707106781186548,-0.707106781186548));
#13799=DIRECTION('',(1.,0.,0.));
#13800=DIRECTION('',(1.,0.,0.));
#13801=DIRECTION('center_axis',(-0.923879532511286,0.,-0.382683432365091));
#13802=DIRECTION('ref_axis',(-0.382683432365091,0.,0.923879532511286));
#13803=DIRECTION('',(0.336556770590779,-0.475963149477967,-0.812519920068745));
#13804=DIRECTION('',(0.,-1.,0.));
#13805=DIRECTION('',(-0.336556770590779,-0.475963149477967,0.812519920068745));
#13806=DIRECTION('',(0.357406744336594,0.357406744336594,-0.862856209461016));
#13807=DIRECTION('center_axis',(-0.577350269189626,-0.577350269189626,-0.577350269189626));
#13808=DIRECTION('ref_axis',(-0.707106781186548,0.,0.707106781186547));
#13809=DIRECTION('',(-0.707106781186548,0.,0.707106781186547));
#13810=DIRECTION('',(-0.812519920068746,0.475963149477963,0.336556770590782));
#13811=DIRECTION('',(0.,0.707106781186548,-0.707106781186548));
#13812=DIRECTION('',(0.475963149477967,0.336556770590778,-0.812519920068745));
#13813=DIRECTION('',(0.812519920068746,-0.336556770590782,-0.475963149477963));
#13814=DIRECTION('center_axis',(-0.382683432365094,0.,-0.923879532511285));
#13815=DIRECTION('ref_axis',(-0.923879532511285,0.,0.382683432365094));
#13816=DIRECTION('',(0.,1.,0.));
#13817=DIRECTION('',(0.812519920068746,0.475963149477963,-0.336556770590782));
#13818=DIRECTION('',(0.862856209461014,-0.357406744336597,-0.357406744336597));
#13819=DIRECTION('',(0.,-1.,0.));
#13820=DIRECTION('',(-0.862856209461014,-0.357406744336597,0.357406744336597));
#13821=DIRECTION('center_axis',(0.,0.,-1.));
#13822=DIRECTION('ref_axis',(-1.,0.,0.));
#13823=DIRECTION('',(-1.,0.,0.));
#13824=DIRECTION('',(0.,1.,0.));
#13825=DIRECTION('',(1.,0.,0.));
#13826=DIRECTION('center_axis',(0.,0.707106781186548,-0.707106781186548));
#13827=DIRECTION('ref_axis',(-1.,0.,0.));
#13828=DIRECTION('',(0.,0.707106781186548,0.707106781186548));
#13829=DIRECTION('',(-1.,0.,0.));
#13830=DIRECTION('',(0.,-0.707106781186548,-0.707106781186548));
#13831=DIRECTION('',(0.862856209461015,0.357406744336595,0.357406744336595));
#13832=DIRECTION('center_axis',(-0.577350269189626,0.577350269189626,-0.577350269189626));
#13833=DIRECTION('ref_axis',(-0.707106781186548,0.,0.707106781186547));
#13834=DIRECTION('',(-0.707106781186548,-0.707106781186548,0.));
#13835=DIRECTION('',(-0.812519920068746,-0.336556770590782,0.475963149477963));
#13836=DIRECTION('',(-0.475963149477968,0.336556770590778,0.812519920068745));
#13837=DIRECTION('',(0.707106781186548,0.,-0.707106781186547));
#13838=DIRECTION('center_axis',(0.382683432365092,0.,-0.923879532511286));
#13839=DIRECTION('ref_axis',(-0.923879532511286,0.,-0.382683432365092));
#13840=DIRECTION('',(0.812519920068746,-0.475963149477966,0.33655677059078));
#13841=DIRECTION('',(0.,-1.,0.));
#13842=DIRECTION('',(-0.812519920068746,-0.475963149477966,-0.33655677059078));
#13843=DIRECTION('',(-0.862856209461015,0.357406744336595,-0.357406744336595));
#13844=DIRECTION('center_axis',(0.,-0.707106781186548,-0.707106781186548));
#13845=DIRECTION('ref_axis',(-1.,0.,0.));
#13846=DIRECTION('',(0.,-0.707106781186548,0.707106781186548));
#13847=DIRECTION('',(1.,0.,0.));
#13848=DIRECTION('center_axis',(0.577350269189626,-0.577350269189626,-0.577350269189626));
#13849=DIRECTION('ref_axis',(-0.707106781186548,0.,-0.707106781186548));
#13850=DIRECTION('',(-0.707106781186548,0.,-0.707106781186548));
#13851=DIRECTION('',(-0.336556770590779,0.475963149477967,-0.812519920068746));
#13852=DIRECTION('',(0.707106781186548,0.707106781186548,0.));
#13853=DIRECTION('',(0.812519920068746,0.336556770590778,0.475963149477968));
#13854=DIRECTION('',(0.475963149477967,-0.336556770590778,0.812519920068745));
#13855=DIRECTION('center_axis',(0.923879532511286,0.,-0.382683432365091));
#13856=DIRECTION('ref_axis',(-0.382683432365091,0.,-0.923879532511286));
#13857=DIRECTION('',(0.,1.,0.));
#13858=DIRECTION('',(0.336556770590779,0.475963149477967,0.812519920068746));
#13859=DIRECTION('',(0.357406744336594,-0.357406744336594,0.862856209461016));
#13860=DIRECTION('',(0.,-1.,0.));
#13861=DIRECTION('',(-0.357406744336594,-0.357406744336594,-0.862856209461016));
#13862=DIRECTION('center_axis',(1.,0.,0.));
#13863=DIRECTION('ref_axis',(0.,0.,-1.));
#13864=DIRECTION('',(0.,0.,-1.));
#13865=DIRECTION('center_axis',(1.,0.,0.));
#13866=DIRECTION('ref_axis',(0.,0.707106781186547,-0.707106781186548));
#13867=DIRECTION('',(0.,1.,0.));
#13868=DIRECTION('center_axis',(1.,0.,0.));
#13869=DIRECTION('ref_axis',(0.,-0.707106781186547,-0.707106781186548));
#13870=DIRECTION('',(0.,0.,1.));
#13871=DIRECTION('center_axis',(-1.,0.,0.));
#13872=DIRECTION('ref_axis',(0.,0.,1.));
#13873=DIRECTION('center_axis',(0.707106781186548,0.707106781186548,0.));
#13874=DIRECTION('ref_axis',(0.,0.,-1.));
#13875=DIRECTION('',(-0.707106781186548,0.707106781186548,0.));
#13876=DIRECTION('',(0.,0.,-1.));
#13877=DIRECTION('',(0.707106781186548,-0.707106781186548,0.));
#13878=DIRECTION('center_axis',(0.577350269189626,0.577350269189626,-0.577350269189626));
#13879=DIRECTION('ref_axis',(-0.707106781186548,0.,-0.707106781186548));
#13880=DIRECTION('',(-0.475963149477967,-0.336556770590778,-0.812519920068745));
#13881=DIRECTION('',(-0.812519920068746,0.336556770590778,-0.475963149477968));
#13882=DIRECTION('',(0.707106781186548,0.,0.707106781186548));
#13883=DIRECTION('center_axis',(0.,-0.923879532511287,-0.382683432365091));
#13884=DIRECTION('ref_axis',(0.,0.382683432365091,-0.923879532511287));
#13885=DIRECTION('',(-0.678598344545847,-0.281084637714821,0.678598344545847));
#13886=DIRECTION('',(-1.,0.,0.));
#13887=DIRECTION('',(-0.678598344545843,0.281084637714822,-0.67859834454585));
#13888=DIRECTION('center_axis',(0.38268343236509,-0.923879532511287,0.));
#13889=DIRECTION('ref_axis',(0.,0.,-1.));
#13890=DIRECTION('',(0.,0.,1.));
#13891=DIRECTION('',(0.923879532511287,0.38268343236509,0.));
#13892=DIRECTION('',(0.,0.,-1.));
#13893=DIRECTION('center_axis',(0.,-1.,0.));
#13894=DIRECTION('ref_axis',(0.,0.,-1.));
#13895=DIRECTION('',(-1.,0.,0.));
#13896=DIRECTION('',(0.,0.,1.));
#13897=DIRECTION('',(-1.,0.,0.));
#13898=DIRECTION('',(0.,0.,-1.));
#13899=DIRECTION('',(1.,0.,0.));
#13900=DIRECTION('',(0.,0.,1.));
#13901=DIRECTION('center_axis',(0.,-1.,0.));
#13902=DIRECTION('ref_axis',(1.,0.,0.));
#13903=DIRECTION('center_axis',(0.,-1.,0.));
#13904=DIRECTION('ref_axis',(1.,0.,0.));
#13905=DIRECTION('center_axis',(0.,-1.,0.));
#13906=DIRECTION('ref_axis',(1.,0.,0.));
#13907=DIRECTION('center_axis',(0.,-1.,0.));
#13908=DIRECTION('ref_axis',(1.,0.,0.));
#13909=DIRECTION('',(-0.707106781186548,-0.707106781186548,0.));
#13910=DIRECTION('',(0.71458114110686,0.699552566126676,7.76834820259501E-15));
#13911=DIRECTION('center_axis',(0.,-0.923879532511286,0.382683432365091));
#13912=DIRECTION('ref_axis',(0.,-0.382683432365091,-0.923879532511286));
#13913=DIRECTION('',(0.678598344545843,-0.281084637714822,-0.67859834454585));
#13914=DIRECTION('',(0.678598344545843,0.281084637714822,0.67859834454585));
#13915=DIRECTION('center_axis',(-0.382683432365094,-0.923879532511285,0.));
#13916=DIRECTION('ref_axis',(0.,0.,-1.));
#13917=DIRECTION('center_axis',(0.,-0.923879532511287,-0.382683432365091));
#13918=DIRECTION('ref_axis',(0.,0.382683432365091,-0.923879532511287));
#13919=DIRECTION('',(-0.678598344545843,-0.281084637714822,0.67859834454585));
#13920=DIRECTION('',(-0.678598344545847,0.281084637714821,-0.678598344545847));
#13921=DIRECTION('center_axis',(0.382683432365094,-0.923879532511285,0.));
#13922=DIRECTION('ref_axis',(0.,0.,-1.));
#13923=DIRECTION('center_axis',(-0.38268343236509,-0.923879532511287,0.));
#13924=DIRECTION('ref_axis',(0.,0.,-1.));
#13925=DIRECTION('',(-0.923879532511287,0.38268343236509,0.));
#13926=DIRECTION('center_axis',(0.,0.923879532511287,-0.382683432365091));
#13927=DIRECTION('ref_axis',(0.,0.382683432365091,0.923879532511287));
#13928=DIRECTION('',(0.678598344545847,0.281084637714821,0.678598344545847));
#13929=DIRECTION('',(1.,0.,0.));
#13930=DIRECTION('',(0.678598344545843,-0.281084637714822,-0.67859834454585));
#13931=DIRECTION('center_axis',(-0.38268343236509,0.923879532511287,0.));
#13932=DIRECTION('ref_axis',(0.,0.,1.));
#13933=DIRECTION('',(0.,0.,1.));
#13934=DIRECTION('',(-0.923879532511287,-0.38268343236509,0.));
#13935=DIRECTION('',(0.,0.,-1.));
#13936=DIRECTION('center_axis',(0.,1.,0.));
#13937=DIRECTION('ref_axis',(0.,0.,1.));
#13938=DIRECTION('',(1.,0.,0.));
#13939=DIRECTION('',(0.,0.,1.));
#13940=DIRECTION('',(1.,0.,0.));
#13941=DIRECTION('',(0.,0.,-1.));
#13942=DIRECTION('',(-1.,0.,0.));
#13943=DIRECTION('',(0.,0.,1.));
#13944=DIRECTION('center_axis',(0.,1.,0.));
#13945=DIRECTION('ref_axis',(1.,0.,0.));
#13946=DIRECTION('center_axis',(0.,1.,0.));
#13947=DIRECTION('ref_axis',(1.,0.,0.));
#13948=DIRECTION('center_axis',(0.,1.,0.));
#13949=DIRECTION('ref_axis',(1.,0.,0.));
#13950=DIRECTION('center_axis',(0.,1.,0.));
#13951=DIRECTION('ref_axis',(1.,0.,0.));
#13952=DIRECTION('',(0.707106781186548,0.707106781186548,0.));
#13953=DIRECTION('',(-0.71458114110686,-0.699552566126676,0.));
#13954=DIRECTION('center_axis',(0.,0.923879532511286,0.382683432365091));
#13955=DIRECTION('ref_axis',(0.,-0.382683432365091,0.923879532511286));
#13956=DIRECTION('',(0.475963149477975,0.336556770590777,-0.812519920068742));
#13957=DIRECTION('',(-0.678598344545843,0.281084637714822,-0.67859834454585));
#13958=DIRECTION('',(-0.678598344545843,-0.281084637714822,0.67859834454585));
#13959=DIRECTION('center_axis',(0.382683432365094,0.923879532511285,0.));
#13960=DIRECTION('ref_axis',(0.,0.,1.));
#13961=DIRECTION('',(0.812519920068753,-0.336556770590785,-0.47596314947795));
#13962=DIRECTION('center_axis',(0.577350269189617,0.57735026918963,0.57735026918963));
#13963=DIRECTION('ref_axis',(0.707106781186555,0.,-0.70710678118654));
#13964=DIRECTION('center_axis',(0.,0.923879532511287,-0.382683432365091));
#13965=DIRECTION('ref_axis',(0.,0.382683432365091,0.923879532511287));
#13966=DIRECTION('',(0.678598344545843,0.281084637714822,0.67859834454585));
#13967=DIRECTION('',(0.678598344545847,-0.281084637714821,-0.678598344545847));
#13968=DIRECTION('center_axis',(-0.382683432365094,0.923879532511285,0.));
#13969=DIRECTION('ref_axis',(0.,0.,1.));
#13970=DIRECTION('',(0.,0.,1.));
#13971=DIRECTION('center_axis',(0.38268343236509,0.923879532511287,0.));
#13972=DIRECTION('ref_axis',(0.,0.,1.));
#13973=DIRECTION('',(0.923879532511287,-0.38268343236509,0.));
#13974=DIRECTION('center_axis',(0.,1.,0.));
#13975=DIRECTION('ref_axis',(1.,0.,0.));
#13976=DIRECTION('',(0.707106781186545,-0.70710678118655,-8.6595605623549E-17));
#13977=DIRECTION('center_axis',(0.,-1.,0.));
#13978=DIRECTION('ref_axis',(1.,0.,0.));
#13979=DIRECTION('center_axis',(0.,1.,0.));
#13980=DIRECTION('ref_axis',(1.,0.,0.));
#13981=DIRECTION('center_axis',(0.,1.,0.));
#13982=DIRECTION('ref_axis',(1.,0.,0.));
#13983=DIRECTION('',(0.,1.,0.));
#13984=DIRECTION('center_axis',(0.,-1.,0.));
#13985=DIRECTION('ref_axis',(1.,0.,0.));
#13986=DIRECTION('',(0.707106781186545,0.70710678118655,8.6595605623549E-17));
#13987=DIRECTION('center_axis',(0.,1.,0.));
#13988=DIRECTION('ref_axis',(1.,0.,0.));
#13989=DIRECTION('',(0.707106781186545,-0.70710678118655,-8.6595605623549E-17));
#13990=DIRECTION('center_axis',(0.,-1.,0.));
#13991=DIRECTION('ref_axis',(1.,0.,0.));
#13992=DIRECTION('center_axis',(0.,1.,0.));
#13993=DIRECTION('ref_axis',(1.,0.,0.));
#13994=DIRECTION('center_axis',(0.,1.,0.));
#13995=DIRECTION('ref_axis',(1.,0.,0.));
#13996=DIRECTION('',(0.,1.,0.));
#13997=DIRECTION('center_axis',(0.,-1.,0.));
#13998=DIRECTION('ref_axis',(1.,0.,0.));
#13999=DIRECTION('',(0.707106781186545,0.70710678118655,8.6595605623549E-17));
#14000=DIRECTION('center_axis',(0.,1.,0.));
#14001=DIRECTION('ref_axis',(1.,0.,0.));
#14002=DIRECTION('',(0.707106781186545,-0.70710678118655,-8.6595605623549E-17));
#14003=DIRECTION('center_axis',(0.,-1.,0.));
#14004=DIRECTION('ref_axis',(1.,0.,0.));
#14005=DIRECTION('center_axis',(0.,1.,0.));
#14006=DIRECTION('ref_axis',(1.,0.,0.));
#14007=DIRECTION('center_axis',(0.,1.,0.));
#14008=DIRECTION('ref_axis',(1.,0.,0.));
#14009=DIRECTION('',(0.,1.,0.));
#14010=DIRECTION('center_axis',(0.,-1.,0.));
#14011=DIRECTION('ref_axis',(1.,0.,0.));
#14012=DIRECTION('',(0.707106781186545,0.70710678118655,8.6595605623549E-17));
#14013=DIRECTION('center_axis',(0.,1.,0.));
#14014=DIRECTION('ref_axis',(1.,0.,0.));
#14015=DIRECTION('',(0.707106781186545,-0.70710678118655,-8.6595605623549E-17));
#14016=DIRECTION('center_axis',(0.,-1.,0.));
#14017=DIRECTION('ref_axis',(1.,0.,0.));
#14018=DIRECTION('center_axis',(0.,1.,0.));
#14019=DIRECTION('ref_axis',(1.,0.,0.));
#14020=DIRECTION('center_axis',(0.,1.,0.));
#14021=DIRECTION('ref_axis',(1.,0.,0.));
#14022=DIRECTION('',(0.,1.,0.));
#14023=DIRECTION('center_axis',(0.,-1.,0.));
#14024=DIRECTION('ref_axis',(1.,0.,0.));
#14025=DIRECTION('',(0.707106781186545,0.70710678118655,8.6595605623549E-17));
#14026=DIRECTION('center_axis',(0.,0.,-1.));
#14027=DIRECTION('ref_axis',(1.,0.,0.));
#14028=DIRECTION('center_axis',(0.,0.,1.));
#14029=DIRECTION('ref_axis',(1.,0.,0.));
#14030=DIRECTION('',(0.707106781186548,8.65956056235494E-17,0.707106781186547));
#14031=DIRECTION('center_axis',(0.,0.,1.));
#14032=DIRECTION('ref_axis',(1.,0.,0.));
#14033=DIRECTION('center_axis',(0.,0.,1.));
#14034=DIRECTION('ref_axis',(1.,0.,0.));
#14035=DIRECTION('',(0.,0.,1.));
#14036=DIRECTION('center_axis',(0.,0.,1.));
#14037=DIRECTION('ref_axis',(1.,0.,0.));
#14038=DIRECTION('center_axis',(0.,0.,1.));
#14039=DIRECTION('ref_axis',(1.,0.,0.));
#14040=DIRECTION('center_axis',(0.,0.,1.));
#14041=DIRECTION('ref_axis',(1.,0.,0.));
#14042=DIRECTION('center_axis',(0.,0.,1.));
#14043=DIRECTION('ref_axis',(1.,0.,0.));
#14044=DIRECTION('',(0.,0.,1.));
#14045=DIRECTION('center_axis',(0.,0.,1.));
#14046=DIRECTION('ref_axis',(1.,0.,0.));
#14047=DIRECTION('center_axis',(0.,0.,-1.));
#14048=DIRECTION('ref_axis',(-1.,0.,0.));
#14049=DIRECTION('center_axis',(0.,0.,1.));
#14050=DIRECTION('ref_axis',(1.,0.,0.));
#14051=DIRECTION('center_axis',(0.,0.,1.));
#14052=DIRECTION('ref_axis',(1.,0.,0.));
#14053=DIRECTION('',(0.,0.,1.));
#14054=DIRECTION('center_axis',(0.,0.,1.));
#14055=DIRECTION('ref_axis',(1.,0.,0.));
#14056=DIRECTION('center_axis',(0.,0.,1.));
#14057=DIRECTION('ref_axis',(1.,0.,0.));
#14058=DIRECTION('',(-0.707106781186542,-8.65956056235487E-17,0.707106781186553));
#14059=DIRECTION('center_axis',(0.,0.,-1.));
#14060=DIRECTION('ref_axis',(1.,0.,0.));
#14061=DIRECTION('center_axis',(1.,0.,0.));
#14062=DIRECTION('ref_axis',(0.,0.,1.));
#14063=DIRECTION('',(-0.707106781186546,8.65956056235495E-17,0.707106781186549));
#14064=DIRECTION('center_axis',(-1.,0.,0.));
#14065=DIRECTION('ref_axis',(0.,0.,1.));
#14066=DIRECTION('center_axis',(-1.,0.,0.));
#14067=DIRECTION('ref_axis',(0.,0.,1.));
#14068=DIRECTION('',(-1.,0.,0.));
#14069=DIRECTION('center_axis',(-1.,0.,0.));
#14070=DIRECTION('ref_axis',(0.,0.,1.));
#14071=DIRECTION('center_axis',(-1.,0.,0.));
#14072=DIRECTION('ref_axis',(0.,0.,1.));
#14073=DIRECTION('center_axis',(-1.,0.,0.));
#14074=DIRECTION('ref_axis',(0.,0.,1.));
#14075=DIRECTION('center_axis',(-1.,0.,0.));
#14076=DIRECTION('ref_axis',(0.,0.,1.));
#14077=DIRECTION('',(-1.,0.,0.));
#14078=DIRECTION('center_axis',(-1.,0.,0.));
#14079=DIRECTION('ref_axis',(0.,0.,1.));
#14080=DIRECTION('center_axis',(1.,0.,0.));
#14081=DIRECTION('ref_axis',(0.,0.,-1.));
#14082=DIRECTION('center_axis',(-1.,0.,0.));
#14083=DIRECTION('ref_axis',(0.,0.,1.));
#14084=DIRECTION('center_axis',(-1.,0.,0.));
#14085=DIRECTION('ref_axis',(0.,0.,1.));
#14086=DIRECTION('',(-1.,0.,0.));
#14087=DIRECTION('center_axis',(-1.,0.,0.));
#14088=DIRECTION('ref_axis',(0.,0.,1.));
#14089=DIRECTION('center_axis',(-1.,0.,0.));
#14090=DIRECTION('ref_axis',(0.,0.,1.));
#14091=DIRECTION('',(-0.707106781186544,-8.65956056235497E-17,-0.707106781186551));
#14092=DIRECTION('center_axis',(1.,0.,0.));
#14093=DIRECTION('ref_axis',(0.,0.,1.));
#14094=DIRECTION('',(-0.707106781186544,8.65956056235497E-17,0.707106781186551));
#14095=DIRECTION('center_axis',(-1.,0.,0.));
#14096=DIRECTION('ref_axis',(0.,0.,1.));
#14097=DIRECTION('center_axis',(-1.,0.,0.));
#14098=DIRECTION('ref_axis',(0.,0.,1.));
#14099=DIRECTION('',(-1.,0.,0.));
#14100=DIRECTION('center_axis',(-1.,0.,0.));
#14101=DIRECTION('ref_axis',(0.,0.,1.));
#14102=DIRECTION('center_axis',(-1.,0.,0.));
#14103=DIRECTION('ref_axis',(0.,0.,1.));
#14104=DIRECTION('center_axis',(-1.,0.,0.));
#14105=DIRECTION('ref_axis',(0.,0.,1.));
#14106=DIRECTION('center_axis',(-1.,0.,0.));
#14107=DIRECTION('ref_axis',(0.,0.,1.));
#14108=DIRECTION('',(-1.,0.,0.));
#14109=DIRECTION('center_axis',(-1.,0.,0.));
#14110=DIRECTION('ref_axis',(0.,0.,1.));
#14111=DIRECTION('center_axis',(1.,0.,0.));
#14112=DIRECTION('ref_axis',(0.,0.,-1.));
#14113=DIRECTION('center_axis',(-1.,0.,0.));
#14114=DIRECTION('ref_axis',(0.,0.,1.));
#14115=DIRECTION('center_axis',(-1.,0.,0.));
#14116=DIRECTION('ref_axis',(0.,0.,1.));
#14117=DIRECTION('',(-1.,0.,0.));
#14118=DIRECTION('center_axis',(-1.,0.,0.));
#14119=DIRECTION('ref_axis',(0.,0.,1.));
#14120=DIRECTION('center_axis',(-1.,0.,0.));
#14121=DIRECTION('ref_axis',(0.,0.,1.));
#14122=DIRECTION('',(-0.707106781186546,-8.65956056235495E-17,-0.707106781186549));
#14123=DIRECTION('center_axis',(0.707106781186548,0.,-0.707106781186548));
#14124=DIRECTION('ref_axis',(-0.707106781186548,0.,-0.707106781186548));
#14125=DIRECTION('center_axis',(-0.707106781186547,0.,-0.707106781186548));
#14126=DIRECTION('ref_axis',(-0.707106781186548,0.,0.707106781186547));
#14127=DIRECTION('center_axis',(0.707106781186548,0.,-0.707106781186548));
#14128=DIRECTION('ref_axis',(-0.707106781186548,0.,-0.707106781186548));
#14129=DIRECTION('center_axis',(-0.707106781186547,0.,-0.707106781186548));
#14130=DIRECTION('ref_axis',(-0.707106781186548,0.,0.707106781186547));
#14131=DIRECTION('center_axis',(-0.707106781186548,0.707106781186548,0.));
#14132=DIRECTION('ref_axis',(0.,0.,1.));
#14133=DIRECTION('center_axis',(-0.707106781186548,0.707106781186548,0.));
#14134=DIRECTION('ref_axis',(0.,0.,1.));
#14135=DIRECTION('center_axis',(0.707106781186548,-0.707106781186548,0.));
#14136=DIRECTION('ref_axis',(0.,0.,-1.));
#14137=DIRECTION('',(0.714581141106858,-0.699552566126678,0.));
#14138=DIRECTION('',(-0.714581141106858,0.699552566126678,0.));
#14139=DIRECTION('center_axis',(1.,0.,0.));
#14140=DIRECTION('ref_axis',(0.,0.,-1.));
#14141=DIRECTION('center_axis',(0.,1.,0.));
#14142=DIRECTION('ref_axis',(-1.,0.,0.));
#14143=DIRECTION('center_axis',(-1.,0.,0.));
#14144=DIRECTION('ref_axis',(0.,-0.707106781186547,-0.707106781186548));
#14145=DIRECTION('center_axis',(1.,0.,0.));
#14146=DIRECTION('ref_axis',(0.,0.,-1.));
#14147=DIRECTION('center_axis',(-1.,0.,0.));
#14148=DIRECTION('ref_axis',(0.,0.707106781186547,-0.707106781186548));
#14149=DIRECTION('center_axis',(0.,1.,0.));
#14150=DIRECTION('ref_axis',(-1.,0.,0.));
#14151=DIRECTION('center_axis',(0.,0.,1.));
#14152=DIRECTION('ref_axis',(1.,0.,0.));
#14153=DIRECTION('center_axis',(-1.,0.,0.));
#14154=DIRECTION('ref_axis',(0.,0.,1.));
#14155=DIRECTION('center_axis',(0.,-1.,0.));
#14156=DIRECTION('ref_axis',(1.,0.,0.));
#14157=DIRECTION('center_axis',(1.,0.,0.));
#14158=DIRECTION('ref_axis',(0.,0.707106781186547,-0.707106781186548));
#14159=DIRECTION('center_axis',(0.,1.,0.));
#14160=DIRECTION('ref_axis',(0.707106781186547,0.,0.707106781186547));
#14161=DIRECTION('center_axis',(0.,-1.,0.));
#14162=DIRECTION('ref_axis',(1.,0.,0.));
#14163=DIRECTION('',(0.,1.,0.));
#14164=DIRECTION('center_axis',(-1.,0.,0.));
#14165=DIRECTION('ref_axis',(0.,0.,1.));
#14166=DIRECTION('center_axis',(1.,0.,0.));
#14167=DIRECTION('ref_axis',(0.,-0.707106781186547,-0.707106781186548));
#14168=DIRECTION('center_axis',(0.,1.,0.));
#14169=DIRECTION('ref_axis',(-0.707106781186547,0.,0.707106781186547));
#14170=DIRECTION('',(0.,-1.,0.));
#14171=DIRECTION('center_axis',(-1.,0.,0.));
#14172=DIRECTION('ref_axis',(0.,0.707106781186547,-0.707106781186547));
#14173=DIRECTION('',(-1.,0.,0.));
#14174=DIRECTION('center_axis',(0.,0.,-1.));
#14175=DIRECTION('ref_axis',(-1.,0.,0.));
#14176=DIRECTION('',(1.,0.,0.));
#14177=DIRECTION('center_axis',(1.,0.,0.));
#14178=DIRECTION('ref_axis',(0.,-0.707106781186547,-0.707106781186547));
#14179=DIRECTION('axis',(0.,0.,1.));
#14180=DIRECTION('refdir',(1.,0.,0.));
#14181=DIRECTION('center_axis',(0.,-2.48590929741675E-15,-1.));
#14182=DIRECTION('ref_axis',(-1.,-3.15543818946224E-17,0.));
#14183=DIRECTION('center_axis',(0.,0.,-1.));
#14184=DIRECTION('ref_axis',(-1.,0.,0.));
#14185=DIRECTION('',(0.923879532511287,-8.09021243661474E-16,-0.382683432365089));
#14186=DIRECTION('center_axis',(0.,0.,1.));
#14187=DIRECTION('ref_axis',(-1.,-6.12323399573677E-17,0.));
#14188=DIRECTION('center_axis',(0.,0.,1.));
#14189=DIRECTION('ref_axis',(-1.,-6.12323399573677E-17,0.));
#14190=DIRECTION('center_axis',(0.,0.,-1.));
#14191=DIRECTION('ref_axis',(1.,0.,0.));
#14192=DIRECTION('',(-0.707106781186548,-8.65956056235493E-17,-0.707106781186548));
#14193=DIRECTION('center_axis',(0.,0.,1.));
#14194=DIRECTION('ref_axis',(1.,0.,0.));
#14195=DIRECTION('center_axis',(0.,0.,1.));
#14196=DIRECTION('ref_axis',(1.,0.,0.));
#14197=DIRECTION('center_axis',(0.,0.,1.));
#14198=DIRECTION('ref_axis',(1.,0.,0.));
#14199=DIRECTION('center_axis',(0.,0.,1.));
#14200=DIRECTION('ref_axis',(1.,0.,0.));
#14201=DIRECTION('center_axis',(0.,0.,1.));
#14202=DIRECTION('ref_axis',(1.,0.,0.));
#14203=DIRECTION('center_axis',(0.,0.,1.));
#14204=DIRECTION('ref_axis',(1.,0.,0.));
#14205=DIRECTION('center_axis',(0.,0.,1.));
#14206=DIRECTION('ref_axis',(1.,0.,0.));
#14207=DIRECTION('center_axis',(0.,0.,1.));
#14208=DIRECTION('ref_axis',(1.,0.,0.));
#14209=DIRECTION('center_axis',(0.,0.,1.));
#14210=DIRECTION('ref_axis',(1.,0.,0.));
#14211=DIRECTION('center_axis',(0.,0.,1.));
#14212=DIRECTION('ref_axis',(1.,0.,0.));
#14213=DIRECTION('center_axis',(0.,0.,1.));
#14214=DIRECTION('ref_axis',(1.,0.,0.));
#14215=DIRECTION('center_axis',(0.,0.,1.));
#14216=DIRECTION('ref_axis',(1.,0.,0.));
#14217=DIRECTION('center_axis',(0.,0.,1.));
#14218=DIRECTION('ref_axis',(1.,0.,0.));
#14219=DIRECTION('center_axis',(0.,0.,1.));
#14220=DIRECTION('ref_axis',(1.,0.,0.));
#14221=DIRECTION('center_axis',(0.,0.,1.));
#14222=DIRECTION('ref_axis',(1.,0.,0.));
#14223=DIRECTION('center_axis',(0.,0.,1.));
#14224=DIRECTION('ref_axis',(1.,0.,0.));
#14225=DIRECTION('center_axis',(0.,0.,1.));
#14226=DIRECTION('ref_axis',(1.,0.,0.));
#14227=DIRECTION('center_axis',(0.,0.,1.));
#14228=DIRECTION('ref_axis',(1.,0.,0.));
#14229=DIRECTION('center_axis',(0.,0.,1.));
#14230=DIRECTION('ref_axis',(1.,0.,0.));
#14231=DIRECTION('center_axis',(0.,0.,1.));
#14232=DIRECTION('ref_axis',(1.,0.,0.));
#14233=DIRECTION('center_axis',(0.,0.,1.));
#14234=DIRECTION('ref_axis',(1.,0.,0.));
#14235=DIRECTION('center_axis',(0.,0.,1.));
#14236=DIRECTION('ref_axis',(1.,0.,0.));
#14237=DIRECTION('center_axis',(0.,0.,1.));
#14238=DIRECTION('ref_axis',(1.,0.,0.));
#14239=DIRECTION('center_axis',(0.,0.,1.));
#14240=DIRECTION('ref_axis',(-0.707106781186547,-0.707106781186548,0.));
#14241=DIRECTION('center_axis',(0.,0.,1.));
#14242=DIRECTION('ref_axis',(1.,0.,0.));
#14243=DIRECTION('center_axis',(0.,0.,1.));
#14244=DIRECTION('ref_axis',(1.,0.,0.));
#14245=DIRECTION('center_axis',(0.,0.,1.));
#14246=DIRECTION('ref_axis',(1.,0.,0.));
#14247=DIRECTION('center_axis',(0.,0.,1.));
#14248=DIRECTION('ref_axis',(1.,0.,0.));
#14249=DIRECTION('center_axis',(-1.,0.,0.));
#14250=DIRECTION('ref_axis',(0.,0.,1.));
#14251=DIRECTION('',(-1.,0.,0.));
#14252=DIRECTION('center_axis',(6.12323399573677E-17,1.,0.));
#14253=DIRECTION('ref_axis',(1.7303891563162E-32,0.,1.));
#14254=DIRECTION('',(6.12323399573677E-17,1.,0.));
#14255=DIRECTION('center_axis',(0.,0.,-1.));
#14256=DIRECTION('ref_axis',(1.,0.,0.));
#14257=DIRECTION('center_axis',(0.,0.,1.));
#14258=DIRECTION('ref_axis',(1.,0.,0.));
#14259=DIRECTION('',(-0.707106781186546,-8.65956056235491E-17,-0.707106781186549));
#14260=DIRECTION('center_axis',(0.,0.,1.));
#14261=DIRECTION('ref_axis',(1.,0.,0.));
#14262=DIRECTION('center_axis',(0.,0.,1.));
#14263=DIRECTION('ref_axis',(1.,0.,0.));
#14264=DIRECTION('center_axis',(0.,0.,1.));
#14265=DIRECTION('ref_axis',(1.,0.,0.));
#14266=DIRECTION('center_axis',(0.,0.,1.));
#14267=DIRECTION('ref_axis',(1.,0.,0.));
#14268=DIRECTION('center_axis',(0.,0.,1.));
#14269=DIRECTION('ref_axis',(1.,0.,0.));
#14270=DIRECTION('center_axis',(0.,0.,1.));
#14271=DIRECTION('ref_axis',(1.,0.,0.));
#14272=DIRECTION('center_axis',(0.,0.,1.));
#14273=DIRECTION('ref_axis',(1.,0.,0.));
#14274=DIRECTION('center_axis',(0.,0.,1.));
#14275=DIRECTION('ref_axis',(1.,0.,0.));
#14276=DIRECTION('center_axis',(0.,0.,1.));
#14277=DIRECTION('ref_axis',(1.,0.,0.));
#14278=DIRECTION('center_axis',(0.,0.,1.));
#14279=DIRECTION('ref_axis',(1.,0.,0.));
#14280=DIRECTION('center_axis',(0.,0.,1.));
#14281=DIRECTION('ref_axis',(1.,0.,0.));
#14282=DIRECTION('center_axis',(0.,0.,1.));
#14283=DIRECTION('ref_axis',(1.,0.,0.));
#14284=DIRECTION('center_axis',(0.,0.,1.));
#14285=DIRECTION('ref_axis',(1.,0.,0.));
#14286=DIRECTION('center_axis',(0.,0.,1.));
#14287=DIRECTION('ref_axis',(1.,0.,0.));
#14288=DIRECTION('center_axis',(0.,0.,1.));
#14289=DIRECTION('ref_axis',(1.,0.,0.));
#14290=DIRECTION('center_axis',(0.,0.,1.));
#14291=DIRECTION('ref_axis',(1.,0.,0.));
#14292=DIRECTION('center_axis',(0.,0.,1.));
#14293=DIRECTION('ref_axis',(1.,0.,0.));
#14294=DIRECTION('center_axis',(0.,0.,1.));
#14295=DIRECTION('ref_axis',(1.,0.,0.));
#14296=DIRECTION('center_axis',(0.,0.,1.));
#14297=DIRECTION('ref_axis',(-0.994427391317185,-0.105423732613193,0.));
#14298=DIRECTION('center_axis',(0.,0.,1.));
#14299=DIRECTION('ref_axis',(1.,0.,0.));
#14300=DIRECTION('center_axis',(0.,0.,1.));
#14301=DIRECTION('ref_axis',(1.,0.,0.));
#14302=DIRECTION('center_axis',(0.,0.,1.));
#14303=DIRECTION('ref_axis',(1.,0.,0.));
#14304=DIRECTION('center_axis',(0.,0.,1.));
#14305=DIRECTION('ref_axis',(1.,0.,0.));
#14306=DIRECTION('center_axis',(0.,0.,1.));
#14307=DIRECTION('ref_axis',(1.,0.,0.));
#14308=DIRECTION('center_axis',(0.,0.,1.));
#14309=DIRECTION('ref_axis',(1.,0.,0.));
#14310=DIRECTION('center_axis',(0.,0.,1.));
#14311=DIRECTION('ref_axis',(1.,0.,0.));
#14312=DIRECTION('center_axis',(0.,0.,1.));
#14313=DIRECTION('ref_axis',(1.,0.,0.));
#14314=DIRECTION('center_axis',(0.,0.,1.));
#14315=DIRECTION('ref_axis',(1.,0.,0.));
#14316=DIRECTION('center_axis',(0.,0.,1.));
#14317=DIRECTION('ref_axis',(1.,0.,0.));
#14318=DIRECTION('center_axis',(0.,0.,1.));
#14319=DIRECTION('ref_axis',(1.,0.,0.));
#14320=DIRECTION('center_axis',(0.,0.,1.));
#14321=DIRECTION('ref_axis',(1.,0.,0.));
#14322=DIRECTION('center_axis',(0.,0.,1.));
#14323=DIRECTION('ref_axis',(1.,0.,0.));
#14324=DIRECTION('center_axis',(0.,0.,1.));
#14325=DIRECTION('ref_axis',(1.,0.,0.));
#14326=DIRECTION('center_axis',(0.,0.,1.));
#14327=DIRECTION('ref_axis',(1.,0.,0.));
#14328=DIRECTION('center_axis',(0.,0.,1.));
#14329=DIRECTION('ref_axis',(1.,0.,0.));
#14330=DIRECTION('center_axis',(0.,0.,1.));
#14331=DIRECTION('ref_axis',(1.,0.,0.));
#14332=DIRECTION('center_axis',(0.,0.,1.));
#14333=DIRECTION('ref_axis',(1.,0.,0.));
#14334=DIRECTION('center_axis',(0.,0.,1.));
#14335=DIRECTION('ref_axis',(1.,0.,0.));
#14336=DIRECTION('center_axis',(0.,0.,-1.));
#14337=DIRECTION('ref_axis',(1.,0.,0.));
#14338=DIRECTION('center_axis',(0.,0.,1.));
#14339=DIRECTION('ref_axis',(1.,0.,0.));
#14340=DIRECTION('',(-0.707106781186548,-8.65956056235493E-17,-0.707106781186548));
#14341=DIRECTION('center_axis',(0.,0.,1.));
#14342=DIRECTION('ref_axis',(1.,0.,0.));
#14343=DIRECTION('center_axis',(0.,0.,1.));
#14344=DIRECTION('ref_axis',(1.,0.,0.));
#14345=DIRECTION('center_axis',(0.,0.,1.));
#14346=DIRECTION('ref_axis',(1.,0.,0.));
#14347=DIRECTION('center_axis',(0.,0.,1.));
#14348=DIRECTION('ref_axis',(1.,0.,0.));
#14349=DIRECTION('center_axis',(0.,0.,1.));
#14350=DIRECTION('ref_axis',(1.,0.,0.));
#14351=DIRECTION('',(0.707106781186547,8.65956056235493E-17,-0.707106781186547));
#14352=DIRECTION('center_axis',(0.,0.,1.));
#14353=DIRECTION('ref_axis',(1.,0.,0.));
#14354=DIRECTION('center_axis',(0.,0.,1.));
#14355=DIRECTION('ref_axis',(1.,0.,0.));
#14356=DIRECTION('',(0.,0.,-1.));
#14357=DIRECTION('center_axis',(0.,0.,1.));
#14358=DIRECTION('ref_axis',(1.,0.,0.));
#14359=DIRECTION('center_axis',(0.,0.,-1.));
#14360=DIRECTION('ref_axis',(1.,0.,0.));
#14361=DIRECTION('',(-0.70710678118655,-8.65956056235496E-17,-0.707106781186545));
#14362=DIRECTION('center_axis',(0.,0.,1.));
#14363=DIRECTION('ref_axis',(1.,0.,0.));
#14364=DIRECTION('center_axis',(0.,0.,-1.));
#14365=DIRECTION('ref_axis',(-1.,0.,0.));
#14366=DIRECTION('axis',(0.,0.,1.));
#14367=DIRECTION('refdir',(1.,0.,0.));
#14368=DIRECTION('center_axis',(0.,0.,1.));
#14369=DIRECTION('ref_axis',(-1.,0.,0.));
#14370=DIRECTION('center_axis',(0.,0.,1.));
#14371=DIRECTION('ref_axis',(-1.,0.,0.));
#14372=DIRECTION('',(-0.707106781186555,-8.65956056235503E-17,-0.70710678118654));
#14373=DIRECTION('center_axis',(0.,0.,-1.));
#14374=DIRECTION('ref_axis',(-1.,0.,0.));
#14375=DIRECTION('center_axis',(0.,0.,-1.));
#14376=DIRECTION('ref_axis',(-1.,0.,0.));
#14377=DIRECTION('center_axis',(0.,0.,1.));
#14378=DIRECTION('ref_axis',(1.,0.,0.));
#14379=DIRECTION('center_axis',(0.,0.,1.));
#14380=DIRECTION('ref_axis',(1.,0.,0.));
#14381=DIRECTION('',(0.,0.,1.));
#14382=DIRECTION('center_axis',(0.,0.,1.));
#14383=DIRECTION('ref_axis',(1.,0.,0.));
#14384=DIRECTION('center_axis',(0.,0.,1.));
#14385=DIRECTION('ref_axis',(1.,0.,0.));
#14386=DIRECTION('center_axis',(0.,0.,1.));
#14387=DIRECTION('ref_axis',(1.,0.,0.));
#14388=DIRECTION('',(-0.857492925712549,-1.05012596676537E-16,0.514495755427518));
#14389=DIRECTION('center_axis',(0.,0.,1.));
#14390=DIRECTION('ref_axis',(0.,-1.,0.));
#14391=DIRECTION('center_axis',(0.,0.,1.));
#14392=DIRECTION('ref_axis',(1.,0.,0.));
#14393=DIRECTION('',(-1.,0.,0.));
#14394=DIRECTION('center_axis',(0.,0.,-1.));
#14395=DIRECTION('ref_axis',(0.,1.,0.));
#14396=DIRECTION('center_axis',(0.,0.,-1.));
#14397=DIRECTION('ref_axis',(1.,0.,0.));
#14398=DIRECTION('',(1.,0.,0.));
#14399=DIRECTION('center_axis',(0.,-1.,0.));
#14400=DIRECTION('ref_axis',(0.,0.,-1.));
#14401=DIRECTION('',(0.,0.,1.));
#14402=DIRECTION('',(0.,0.,-1.));
#14403=DIRECTION('center_axis',(0.,0.,-1.));
#14404=DIRECTION('ref_axis',(-1.,0.,0.));
#14405=DIRECTION('center_axis',(0.,0.,-1.));
#14406=DIRECTION('ref_axis',(1.,0.,0.));
#14407=DIRECTION('',(0.,1.,0.));
#14408=DIRECTION('center_axis',(-1.,0.,0.));
#14409=DIRECTION('ref_axis',(0.,0.,1.));
#14410=DIRECTION('',(0.,0.,-1.));
#14411=DIRECTION('',(0.,-1.,0.));
#14412=DIRECTION('',(0.,0.,1.));
#14413=DIRECTION('center_axis',(0.,0.,1.));
#14414=DIRECTION('ref_axis',(1.,0.,0.));
#14415=DIRECTION('center_axis',(0.,0.,1.));
#14416=DIRECTION('ref_axis',(1.,0.,0.));
#14417=DIRECTION('center_axis',(0.,0.,-1.));
#14418=DIRECTION('ref_axis',(-1.,0.,0.));
#14419=DIRECTION('center_axis',(0.,0.,1.));
#14420=DIRECTION('ref_axis',(1.,0.,0.));
#14421=DIRECTION('center_axis',(0.,0.,1.));
#14422=DIRECTION('ref_axis',(1.,0.,0.));
#14423=DIRECTION('center_axis',(0.,0.,1.));
#14424=DIRECTION('ref_axis',(1.,0.,0.));
#14425=DIRECTION('',(0.707106781186547,8.65956056235493E-17,-0.707106781186548));
#14426=DIRECTION('center_axis',(0.,0.,1.));
#14427=DIRECTION('ref_axis',(1.,0.,0.));
#14428=DIRECTION('center_axis',(0.,0.,1.));
#14429=DIRECTION('ref_axis',(1.,0.,0.));
#14430=DIRECTION('',(0.,0.,-1.));
#14431=DIRECTION('center_axis',(0.,0.,1.));
#14432=DIRECTION('ref_axis',(1.,0.,0.));
#14433=DIRECTION('center_axis',(0.,0.,1.));
#14434=DIRECTION('ref_axis',(1.,0.,0.));
#14435=DIRECTION('center_axis',(0.,0.,1.));
#14436=DIRECTION('ref_axis',(1.,0.,0.));
#14437=DIRECTION('center_axis',(0.,0.,1.));
#14438=DIRECTION('ref_axis',(1.,0.,0.));
#14439=DIRECTION('',(0.,0.,-1.));
#14440=DIRECTION('center_axis',(0.,0.,-1.));
#14441=DIRECTION('ref_axis',(-1.,0.,0.));
#14442=DIRECTION('center_axis',(0.,0.,1.));
#14443=DIRECTION('ref_axis',(1.,0.,0.));
#14444=DIRECTION('center_axis',(0.,0.,1.));
#14445=DIRECTION('ref_axis',(1.,0.,0.));
#14446=DIRECTION('center_axis',(0.,0.,1.));
#14447=DIRECTION('ref_axis',(1.,0.,0.));
#14448=DIRECTION('',(0.,0.,-1.));
#14449=DIRECTION('center_axis',(0.,0.,-1.));
#14450=DIRECTION('ref_axis',(1.,0.,0.));
#14451=DIRECTION('',(-0.707106781186542,-8.65956056235487E-17,-0.707106781186553));
#14452=DIRECTION('axis',(0.,0.,1.));
#14453=DIRECTION('refdir',(1.,0.,0.));
#14454=DIRECTION('center_axis',(0.,0.,1.));
#14455=DIRECTION('ref_axis',(-0.707106781186547,-0.707106781186548,0.));
#14456=DIRECTION('center_axis',(0.,0.,1.));
#14457=DIRECTION('ref_axis',(1.,0.,0.));
#14458=DIRECTION('center_axis',(0.,0.,1.));
#14459=DIRECTION('ref_axis',(1.,0.,0.));
#14460=DIRECTION('center_axis',(0.,0.,1.));
#14461=DIRECTION('ref_axis',(1.,0.,0.));
#14462=DIRECTION('center_axis',(0.,0.,1.));
#14463=DIRECTION('ref_axis',(1.,0.,0.));
#14464=DIRECTION('center_axis',(0.,0.,1.));
#14465=DIRECTION('ref_axis',(1.,0.,0.));
#14466=DIRECTION('center_axis',(0.,0.,1.));
#14467=DIRECTION('ref_axis',(1.,0.,0.));
#14468=DIRECTION('center_axis',(-1.,0.,0.));
#14469=DIRECTION('ref_axis',(0.,0.,1.));
#14470=DIRECTION('',(-1.,0.,0.));
#14471=DIRECTION('center_axis',(6.12323399573677E-17,1.,0.));
#14472=DIRECTION('ref_axis',(1.7303891563162E-32,0.,1.));
#14473=DIRECTION('',(6.12323399573677E-17,1.,0.));
#14474=DIRECTION('center_axis',(0.,0.,-1.));
#14475=DIRECTION('ref_axis',(1.,0.,0.));
#14476=DIRECTION('center_axis',(0.,0.,1.));
#14477=DIRECTION('ref_axis',(1.,0.,0.));
#14478=DIRECTION('',(-0.707106781186546,-8.65956056235491E-17,-0.707106781186549));
#14479=DIRECTION('center_axis',(0.,0.,-1.));
#14480=DIRECTION('ref_axis',(1.,0.,0.));
#14481=DIRECTION('center_axis',(0.,0.,1.));
#14482=DIRECTION('ref_axis',(1.,0.,0.));
#14483=DIRECTION('',(-0.707106781186548,-8.65956056235493E-17,-0.707106781186548));
#14484=DIRECTION('center_axis',(0.,0.,1.));
#14485=DIRECTION('ref_axis',(1.,0.,0.));
#14486=DIRECTION('center_axis',(0.,0.,1.));
#14487=DIRECTION('ref_axis',(1.,0.,0.));
#14488=DIRECTION('center_axis',(0.,0.,1.));
#14489=DIRECTION('ref_axis',(1.,0.,0.));
#14490=DIRECTION('center_axis',(0.,0.,1.));
#14491=DIRECTION('ref_axis',(1.,0.,0.));
#14492=DIRECTION('center_axis',(0.,0.,1.));
#14493=DIRECTION('ref_axis',(1.,0.,0.));
#14494=DIRECTION('center_axis',(0.,0.,1.));
#14495=DIRECTION('ref_axis',(1.,0.,0.));
#14496=DIRECTION('center_axis',(0.,0.,1.));
#14497=DIRECTION('ref_axis',(1.,0.,0.));
#14498=DIRECTION('center_axis',(0.,0.,1.));
#14499=DIRECTION('ref_axis',(1.,0.,0.));
#14500=DIRECTION('center_axis',(0.,0.,1.));
#14501=DIRECTION('ref_axis',(1.,0.,0.));
#14502=DIRECTION('center_axis',(0.,0.,1.));
#14503=DIRECTION('ref_axis',(1.,0.,0.));
#14504=DIRECTION('center_axis',(0.,0.,1.));
#14505=DIRECTION('ref_axis',(1.,0.,0.));
#14506=DIRECTION('center_axis',(0.,0.,1.));
#14507=DIRECTION('ref_axis',(1.,0.,0.));
#14508=DIRECTION('center_axis',(0.,0.,1.));
#14509=DIRECTION('ref_axis',(1.,0.,0.));
#14510=DIRECTION('center_axis',(0.,0.,1.));
#14511=DIRECTION('ref_axis',(1.,0.,0.));
#14512=DIRECTION('center_axis',(0.,0.,1.));
#14513=DIRECTION('ref_axis',(1.,0.,0.));
#14514=DIRECTION('center_axis',(0.,0.,1.));
#14515=DIRECTION('ref_axis',(1.,0.,0.));
#14516=DIRECTION('center_axis',(0.,0.,1.));
#14517=DIRECTION('ref_axis',(1.,0.,0.));
#14518=DIRECTION('center_axis',(0.,0.,1.));
#14519=DIRECTION('ref_axis',(1.,0.,0.));
#14520=DIRECTION('center_axis',(0.,0.,1.));
#14521=DIRECTION('ref_axis',(1.,0.,0.));
#14522=DIRECTION('center_axis',(0.,0.,1.));
#14523=DIRECTION('ref_axis',(1.,0.,0.));
#14524=DIRECTION('center_axis',(0.,0.,1.));
#14525=DIRECTION('ref_axis',(1.,0.,0.));
#14526=DIRECTION('center_axis',(0.,0.,1.));
#14527=DIRECTION('ref_axis',(1.,0.,0.));
#14528=DIRECTION('center_axis',(0.,0.,1.));
#14529=DIRECTION('ref_axis',(1.,0.,0.));
#14530=DIRECTION('center_axis',(0.,0.,1.));
#14531=DIRECTION('ref_axis',(1.,0.,0.));
#14532=DIRECTION('center_axis',(0.,0.,1.));
#14533=DIRECTION('ref_axis',(1.,0.,0.));
#14534=DIRECTION('center_axis',(0.,0.,1.));
#14535=DIRECTION('ref_axis',(1.,0.,0.));
#14536=DIRECTION('center_axis',(0.,0.,1.));
#14537=DIRECTION('ref_axis',(1.,0.,0.));
#14538=DIRECTION('center_axis',(0.,0.,1.));
#14539=DIRECTION('ref_axis',(1.,0.,0.));
#14540=DIRECTION('center_axis',(0.,0.,1.));
#14541=DIRECTION('ref_axis',(1.,0.,0.));
#14542=DIRECTION('center_axis',(0.,0.,1.));
#14543=DIRECTION('ref_axis',(1.,0.,0.));
#14544=DIRECTION('center_axis',(0.,0.,1.));
#14545=DIRECTION('ref_axis',(1.,0.,0.));
#14546=DIRECTION('center_axis',(0.,0.,1.));
#14547=DIRECTION('ref_axis',(1.,0.,0.));
#14548=DIRECTION('center_axis',(0.,0.,1.));
#14549=DIRECTION('ref_axis',(1.,0.,0.));
#14550=DIRECTION('center_axis',(0.,0.,1.));
#14551=DIRECTION('ref_axis',(1.,0.,0.));
#14552=DIRECTION('center_axis',(0.,0.,1.));
#14553=DIRECTION('ref_axis',(1.,0.,0.));
#14554=DIRECTION('center_axis',(0.,0.,1.));
#14555=DIRECTION('ref_axis',(1.,0.,0.));
#14556=DIRECTION('center_axis',(0.,0.,1.));
#14557=DIRECTION('ref_axis',(1.,0.,0.));
#14558=DIRECTION('center_axis',(0.,0.,1.));
#14559=DIRECTION('ref_axis',(1.,0.,0.));
#14560=DIRECTION('center_axis',(0.,0.,1.));
#14561=DIRECTION('ref_axis',(1.,0.,0.));
#14562=DIRECTION('center_axis',(0.,0.,1.));
#14563=DIRECTION('ref_axis',(1.,0.,0.));
#14564=DIRECTION('center_axis',(0.,0.,1.));
#14565=DIRECTION('ref_axis',(-0.994427391317185,0.105423732613192,0.));
#14566=DIRECTION('center_axis',(0.,0.,1.));
#14567=DIRECTION('ref_axis',(1.,0.,0.));
#14568=DIRECTION('center_axis',(0.,0.,1.));
#14569=DIRECTION('ref_axis',(1.,0.,0.));
#14570=DIRECTION('center_axis',(0.,0.,1.));
#14571=DIRECTION('ref_axis',(1.,0.,0.));
#14572=DIRECTION('center_axis',(0.,0.,1.));
#14573=DIRECTION('ref_axis',(1.,0.,0.));
#14574=DIRECTION('center_axis',(0.,0.,1.));
#14575=DIRECTION('ref_axis',(1.,0.,0.));
#14576=DIRECTION('center_axis',(0.,0.,1.));
#14577=DIRECTION('ref_axis',(1.,0.,0.));
#14578=DIRECTION('center_axis',(0.,0.,1.));
#14579=DIRECTION('ref_axis',(1.,0.,0.));
#14580=DIRECTION('center_axis',(0.,0.,1.));
#14581=DIRECTION('ref_axis',(1.,0.,0.));
#14582=DIRECTION('center_axis',(0.,0.,1.));
#14583=DIRECTION('ref_axis',(1.,0.,0.));
#14584=DIRECTION('center_axis',(0.,0.,1.));
#14585=DIRECTION('ref_axis',(1.,0.,0.));
#14586=DIRECTION('center_axis',(0.,0.,1.));
#14587=DIRECTION('ref_axis',(1.,0.,0.));
#14588=DIRECTION('center_axis',(0.,0.,1.));
#14589=DIRECTION('ref_axis',(1.,0.,0.));
#14590=DIRECTION('center_axis',(0.,0.,1.));
#14591=DIRECTION('ref_axis',(1.,0.,0.));
#14592=DIRECTION('center_axis',(0.,0.,1.));
#14593=DIRECTION('ref_axis',(1.,0.,0.));
#14594=DIRECTION('center_axis',(0.,0.,1.));
#14595=DIRECTION('ref_axis',(1.,0.,0.));
#14596=DIRECTION('center_axis',(0.,0.,1.));
#14597=DIRECTION('ref_axis',(1.,0.,0.));
#14598=DIRECTION('center_axis',(0.,0.,1.));
#14599=DIRECTION('ref_axis',(1.,0.,0.));
#14600=DIRECTION('center_axis',(0.,0.,-1.));
#14601=DIRECTION('ref_axis',(1.,0.,0.));
#14602=DIRECTION('center_axis',(0.,0.,1.));
#14603=DIRECTION('ref_axis',(1.,0.,0.));
#14604=DIRECTION('',(-0.707106781186548,-8.65956056235493E-17,-0.707106781186548));
#14605=DIRECTION('center_axis',(0.,0.,1.));
#14606=DIRECTION('ref_axis',(1.,0.,0.));
#14607=DIRECTION('center_axis',(0.,0.,1.));
#14608=DIRECTION('ref_axis',(1.,0.,0.));
#14609=DIRECTION('center_axis',(0.,0.,1.));
#14610=DIRECTION('ref_axis',(1.,0.,0.));
#14611=DIRECTION('center_axis',(0.,0.,1.));
#14612=DIRECTION('ref_axis',(1.,0.,0.));
#14613=DIRECTION('center_axis',(0.,0.,1.));
#14614=DIRECTION('ref_axis',(1.,0.,0.));
#14615=DIRECTION('center_axis',(0.,0.,1.));
#14616=DIRECTION('ref_axis',(1.,0.,0.));
#14617=DIRECTION('',(0.707106781186547,8.65956056235493E-17,-0.707106781186547));
#14618=DIRECTION('center_axis',(0.,0.,1.));
#14619=DIRECTION('ref_axis',(1.,0.,0.));
#14620=DIRECTION('center_axis',(0.,0.,1.));
#14621=DIRECTION('ref_axis',(1.,0.,0.));
#14622=DIRECTION('',(0.,0.,-1.));
#14623=DIRECTION('center_axis',(0.,0.,1.));
#14624=DIRECTION('ref_axis',(1.,0.,0.));
#14625=DIRECTION('center_axis',(0.,0.,-1.));
#14626=DIRECTION('ref_axis',(1.,0.,0.));
#14627=DIRECTION('',(-0.70710678118655,-8.65956056235496E-17,-0.707106781186545));
#14628=DIRECTION('center_axis',(0.,0.,1.));
#14629=DIRECTION('ref_axis',(1.,0.,0.));
#14630=DIRECTION('center_axis',(0.,0.,-1.));
#14631=DIRECTION('ref_axis',(-1.,0.,0.));
#14632=DIRECTION('axis',(0.,0.,1.));
#14633=DIRECTION('refdir',(1.,0.,0.));
#14634=DIRECTION('center_axis',(0.,0.,-1.));
#14635=DIRECTION('ref_axis',(-1.,0.,0.));
#14636=DIRECTION('center_axis',(0.,0.,1.));
#14637=DIRECTION('ref_axis',(1.,0.,0.));
#14638=DIRECTION('center_axis',(0.,0.,1.));
#14639=DIRECTION('ref_axis',(1.,0.,0.));
#14640=DIRECTION('center_axis',(0.,0.,1.));
#14641=DIRECTION('ref_axis',(1.,0.,0.));
#14642=DIRECTION('center_axis',(0.,0.,-1.));
#14643=DIRECTION('ref_axis',(1.,0.,0.));
#14644=DIRECTION('center_axis',(0.,0.,1.));
#14645=DIRECTION('ref_axis',(1.,0.,0.));
#14646=DIRECTION('center_axis',(0.,0.,1.));
#14647=DIRECTION('ref_axis',(1.,0.,0.));
#14648=DIRECTION('',(0.,0.,-1.));
#14649=DIRECTION('center_axis',(0.,0.,1.));
#14650=DIRECTION('ref_axis',(1.,0.,0.));
#14651=DIRECTION('center_axis',(0.,0.,1.));
#14652=DIRECTION('ref_axis',(1.,0.,0.));
#14653=DIRECTION('',(0.,0.,-1.));
#14654=DIRECTION('center_axis',(0.,0.,-1.));
#14655=DIRECTION('ref_axis',(-1.,0.,0.));
#14656=DIRECTION('center_axis',(0.,0.,1.));
#14657=DIRECTION('ref_axis',(1.,0.,0.));
#14658=DIRECTION('center_axis',(0.,0.,1.));
#14659=DIRECTION('ref_axis',(1.,0.,0.));
#14660=DIRECTION('center_axis',(0.,0.,1.));
#14661=DIRECTION('ref_axis',(1.,0.,0.));
#14662=DIRECTION('center_axis',(0.,0.,-1.));
#14663=DIRECTION('ref_axis',(1.,0.,0.));
#14664=DIRECTION('center_axis',(0.,0.,1.));
#14665=DIRECTION('ref_axis',(1.,0.,0.));
#14666=DIRECTION('center_axis',(0.,0.,1.));
#14667=DIRECTION('ref_axis',(1.,0.,0.));
#14668=DIRECTION('',(0.,0.,-1.));
#14669=DIRECTION('center_axis',(0.,0.,1.));
#14670=DIRECTION('ref_axis',(1.,0.,0.));
#14671=DIRECTION('center_axis',(0.,0.,1.));
#14672=DIRECTION('ref_axis',(1.,0.,0.));
#14673=DIRECTION('center_axis',(0.,0.,1.));
#14674=DIRECTION('ref_axis',(1.,0.,0.));
#14675=DIRECTION('center_axis',(0.,0.,1.));
#14676=DIRECTION('ref_axis',(1.,0.,0.));
#14677=DIRECTION('center_axis',(0.,0.,1.));
#14678=DIRECTION('ref_axis',(1.,0.,0.));
#14679=DIRECTION('center_axis',(0.,0.,1.));
#14680=DIRECTION('ref_axis',(1.,0.,0.));
#14681=DIRECTION('',(0.,0.,-1.));
#14682=DIRECTION('center_axis',(0.,0.,1.));
#14683=DIRECTION('ref_axis',(1.,0.,0.));
#14684=DIRECTION('center_axis',(0.,0.,1.));
#14685=DIRECTION('ref_axis',(1.,0.,0.));
#14686=DIRECTION('center_axis',(0.,0.,1.));
#14687=DIRECTION('ref_axis',(1.,0.,0.));
#14688=DIRECTION('center_axis',(0.,0.,1.));
#14689=DIRECTION('ref_axis',(0.623489801858733,-0.78183148246803,0.));
#14690=DIRECTION('center_axis',(-0.78183148246803,-0.623489801858733,0.));
#14691=DIRECTION('ref_axis',(-0.623489801858733,0.78183148246803,0.));
#14692=DIRECTION('center_axis',(-0.78183148246803,-0.623489801858733,0.));
#14693=DIRECTION('ref_axis',(-0.623489801858733,0.78183148246803,0.));
#14694=DIRECTION('center_axis',(0.,0.,1.));
#14695=DIRECTION('ref_axis',(1.,0.,0.));
#14696=DIRECTION('',(0.,0.,-1.));
#14697=DIRECTION('center_axis',(0.,0.,-1.));
#14698=DIRECTION('ref_axis',(1.,0.,0.));
#14699=DIRECTION('center_axis',(0.,0.,-1.));
#14700=DIRECTION('ref_axis',(1.,0.,0.));
#14701=DIRECTION('center_axis',(0.,0.,-1.));
#14702=DIRECTION('ref_axis',(1.,0.,0.));
#14703=DIRECTION('center_axis',(0.,0.,-1.));
#14704=DIRECTION('ref_axis',(1.,0.,0.));
#14705=DIRECTION('center_axis',(0.,0.,-1.));
#14706=DIRECTION('ref_axis',(1.,0.,0.));
#14707=DIRECTION('center_axis',(0.,0.,-1.));
#14708=DIRECTION('ref_axis',(1.,0.,0.));
#14709=DIRECTION('center_axis',(0.,0.,-1.));
#14710=DIRECTION('ref_axis',(1.,0.,0.));
#14711=DIRECTION('center_axis',(0.,0.,-1.));
#14712=DIRECTION('ref_axis',(1.,0.,0.));
#14713=DIRECTION('center_axis',(0.,0.,1.));
#14714=DIRECTION('ref_axis',(1.,0.,0.));
#14715=DIRECTION('center_axis',(0.,0.,1.));
#14716=DIRECTION('ref_axis',(1.,0.,0.));
#14717=DIRECTION('center_axis',(0.,0.,-1.));
#14718=DIRECTION('ref_axis',(1.,0.,0.));
#14719=DIRECTION('center_axis',(0.,0.,-1.));
#14720=DIRECTION('ref_axis',(1.,0.,0.));
#14721=DIRECTION('center_axis',(0.,0.,-1.));
#14722=DIRECTION('ref_axis',(1.,0.,0.));
#14723=DIRECTION('',(0.,0.,-1.));
#14724=DIRECTION('center_axis',(0.,0.,1.));
#14725=DIRECTION('ref_axis',(1.,0.,0.));
#14726=DIRECTION('center_axis',(0.,0.,-1.));
#14727=DIRECTION('ref_axis',(1.,0.,0.));
#14728=DIRECTION('center_axis',(0.,0.,-1.));
#14729=DIRECTION('ref_axis',(1.,0.,0.));
#14730=DIRECTION('center_axis',(0.,0.,-1.));
#14731=DIRECTION('ref_axis',(1.,0.,0.));
#14732=DIRECTION('center_axis',(0.,0.,-1.));
#14733=DIRECTION('ref_axis',(1.,0.,0.));
#14734=DIRECTION('center_axis',(0.,0.,-1.));
#14735=DIRECTION('ref_axis',(1.,0.,0.));
#14736=DIRECTION('center_axis',(0.,0.,1.));
#14737=DIRECTION('ref_axis',(1.,0.,0.));
#14738=DIRECTION('center_axis',(0.,0.,1.));
#14739=DIRECTION('ref_axis',(1.,0.,0.));
#14740=DIRECTION('center_axis',(0.,0.,1.));
#14741=DIRECTION('ref_axis',(-0.222520933956315,-0.974927912181824,0.));
#14742=DIRECTION('center_axis',(-0.974927912181824,0.222520933956314,0.));
#14743=DIRECTION('ref_axis',(0.222520933956314,0.974927912181824,0.));
#14744=DIRECTION('center_axis',(-0.974927912181824,0.222520933956314,0.));
#14745=DIRECTION('ref_axis',(0.222520933956314,0.974927912181824,0.));
#14746=DIRECTION('center_axis',(0.,0.,1.));
#14747=DIRECTION('ref_axis',(1.,0.,0.));
#14748=DIRECTION('center_axis',(0.,0.,1.));
#14749=DIRECTION('ref_axis',(1.,0.,0.));
#14750=DIRECTION('center_axis',(0.,0.,1.));
#14751=DIRECTION('ref_axis',(1.,0.,0.));
#14752=DIRECTION('center_axis',(0.,0.,1.));
#14753=DIRECTION('ref_axis',(-0.900968867902419,-0.433883739117558,0.));
#14754=DIRECTION('center_axis',(-0.433883739117558,0.900968867902419,0.));
#14755=DIRECTION('ref_axis',(0.900968867902419,0.433883739117558,0.));
#14756=DIRECTION('center_axis',(-0.433883739117558,0.900968867902419,0.));
#14757=DIRECTION('ref_axis',(0.900968867902419,0.433883739117558,0.));
#14758=DIRECTION('center_axis',(0.,0.,1.));
#14759=DIRECTION('ref_axis',(-1.,-1.22464679914735E-16,0.));
#14760=DIRECTION('center_axis',(0.,0.,1.));
#14761=DIRECTION('ref_axis',(-1.,6.98296267768627E-15,0.));
#14762=DIRECTION('center_axis',(0.,0.,1.));
#14763=DIRECTION('ref_axis',(1.,0.,0.));
#14764=DIRECTION('center_axis',(0.,0.,1.));
#14765=DIRECTION('ref_axis',(1.,0.,0.));
#14766=DIRECTION('center_axis',(0.,0.,1.));
#14767=DIRECTION('ref_axis',(-0.900968867902419,0.433883739117559,0.));
#14768=DIRECTION('center_axis',(0.433883739117558,0.900968867902419,0.));
#14769=DIRECTION('ref_axis',(0.900968867902419,-0.433883739117558,0.));
#14770=DIRECTION('center_axis',(0.433883739117558,0.900968867902419,0.));
#14771=DIRECTION('ref_axis',(0.900968867902419,-0.433883739117558,0.));
#14772=DIRECTION('center_axis',(0.,0.,1.));
#14773=DIRECTION('ref_axis',(1.,0.,0.));
#14774=DIRECTION('center_axis',(0.,0.,1.));
#14775=DIRECTION('ref_axis',(1.,0.,0.));
#14776=DIRECTION('center_axis',(0.,0.,1.));
#14777=DIRECTION('ref_axis',(1.,0.,0.));
#14778=DIRECTION('center_axis',(0.,0.,1.));
#14779=DIRECTION('ref_axis',(-0.222520933956314,0.974927912181824,0.));
#14780=DIRECTION('center_axis',(0.974927912181824,0.222520933956314,0.));
#14781=DIRECTION('ref_axis',(0.222520933956314,-0.974927912181824,0.));
#14782=DIRECTION('center_axis',(0.974927912181824,0.222520933956314,0.));
#14783=DIRECTION('ref_axis',(0.222520933956314,-0.974927912181824,0.));
#14784=DIRECTION('center_axis',(0.,0.,1.));
#14785=DIRECTION('ref_axis',(1.,0.,0.));
#14786=DIRECTION('center_axis',(0.,0.,1.));
#14787=DIRECTION('ref_axis',(1.,0.,0.));
#14788=DIRECTION('center_axis',(0.,0.,1.));
#14789=DIRECTION('ref_axis',(1.,0.,0.));
#14790=DIRECTION('center_axis',(0.,0.,1.));
#14791=DIRECTION('ref_axis',(0.623489801858733,0.78183148246803,0.));
#14792=DIRECTION('center_axis',(0.78183148246803,-0.623489801858733,0.));
#14793=DIRECTION('ref_axis',(-0.623489801858733,-0.78183148246803,0.));
#14794=DIRECTION('center_axis',(0.78183148246803,-0.623489801858733,0.));
#14795=DIRECTION('ref_axis',(-0.623489801858733,-0.78183148246803,0.));
#14796=DIRECTION('center_axis',(0.,0.,1.));
#14797=DIRECTION('ref_axis',(1.,0.,0.));
#14798=DIRECTION('',(0.,0.,-1.));
#14799=DIRECTION('center_axis',(0.,0.,1.));
#14800=DIRECTION('ref_axis',(1.,0.,0.));
#14801=DIRECTION('center_axis',(0.,0.,1.));
#14802=DIRECTION('ref_axis',(1.,0.,0.));
#14803=DIRECTION('center_axis',(0.,0.,1.));
#14804=DIRECTION('ref_axis',(1.,0.,0.));
#14805=DIRECTION('center_axis',(0.,0.,1.));
#14806=DIRECTION('ref_axis',(1.,0.,0.));
#14807=DIRECTION('',(0.,0.,-1.));
#14808=DIRECTION('center_axis',(0.,0.,1.));
#14809=DIRECTION('ref_axis',(1.,0.,0.));
#14810=DIRECTION('center_axis',(0.,0.,1.));
#14811=DIRECTION('ref_axis',(1.,0.,0.));
#14812=DIRECTION('center_axis',(0.,0.,1.));
#14813=DIRECTION('ref_axis',(1.,0.,0.));
#14814=DIRECTION('center_axis',(0.,0.,1.));
#14815=DIRECTION('ref_axis',(1.,0.,0.));
#14816=DIRECTION('center_axis',(1.22464679914735E-16,-1.,0.));
#14817=DIRECTION('ref_axis',(-1.,-1.22464679914735E-16,0.));
#14818=DIRECTION('center_axis',(1.22464679914735E-16,-1.,0.));
#14819=DIRECTION('ref_axis',(-1.,-1.22464679914735E-16,0.));
#14820=DIRECTION('center_axis',(0.,0.,1.));
#14821=DIRECTION('ref_axis',(1.,0.,0.));
#14822=DIRECTION('center_axis',(0.,0.,-1.));
#14823=DIRECTION('ref_axis',(-1.,0.,0.));
#14824=DIRECTION('center_axis',(0.,0.,1.));
#14825=DIRECTION('ref_axis',(1.,0.,0.));
#14826=DIRECTION('center_axis',(0.,0.,1.));
#14827=DIRECTION('ref_axis',(1.,0.,0.));
#14828=DIRECTION('center_axis',(0.,0.,1.));
#14829=DIRECTION('ref_axis',(1.,0.,0.));
#14830=DIRECTION('',(0.70710678118655,8.65956056235497E-17,-0.707106781186545));
#14831=DIRECTION('center_axis',(0.,0.,1.));
#14832=DIRECTION('ref_axis',(1.,0.,0.));
#14833=DIRECTION('center_axis',(0.,0.,1.));
#14834=DIRECTION('ref_axis',(1.,0.,0.));
#14835=DIRECTION('',(0.,0.,-1.));
#14836=DIRECTION('center_axis',(0.,0.,-1.));
#14837=DIRECTION('ref_axis',(1.,0.,0.));
#14838=DIRECTION('center_axis',(0.,0.,1.));
#14839=DIRECTION('ref_axis',(1.,0.,0.));
#14840=DIRECTION('',(-0.70710678118655,-8.65956056235497E-17,-0.707106781186545));
#14841=DIRECTION('center_axis',(0.,0.,1.));
#14842=DIRECTION('ref_axis',(1.,0.,0.));
#14843=DIRECTION('center_axis',(0.,0.,1.));
#14844=DIRECTION('ref_axis',(1.,0.,0.));
#14845=DIRECTION('center_axis',(0.,0.,1.));
#14846=DIRECTION('ref_axis',(1.,0.,0.));
#14847=DIRECTION('center_axis',(0.,0.,1.));
#14848=DIRECTION('ref_axis',(1.,0.,0.));
#14849=DIRECTION('',(0.,0.,-1.));
#14850=DIRECTION('center_axis',(0.,0.,1.));
#14851=DIRECTION('ref_axis',(1.,0.,0.));
#14852=DIRECTION('center_axis',(0.,0.,-1.));
#14853=DIRECTION('ref_axis',(1.,0.,0.));
#14854=DIRECTION('',(-0.70710678118655,-8.65956056235497E-17,-0.707106781186545));
#14855=DIRECTION('center_axis',(0.,0.,1.));
#14856=DIRECTION('ref_axis',(1.,0.,0.));
#14857=DIRECTION('center_axis',(0.,0.,-1.));
#14858=DIRECTION('ref_axis',(-1.,0.,0.));
#14859=DIRECTION('center_axis',(0.,0.,1.));
#14860=DIRECTION('ref_axis',(1.,0.,0.));
#14861=DIRECTION('center_axis',(0.,0.,1.));
#14862=DIRECTION('ref_axis',(1.,0.,0.));
#14863=DIRECTION('center_axis',(0.,0.,1.));
#14864=DIRECTION('ref_axis',(1.,0.,0.));
#14865=DIRECTION('',(0.70710678118655,8.65956056235497E-17,-0.707106781186545));
#14866=DIRECTION('axis',(0.,0.,1.));
#14867=DIRECTION('refdir',(1.,0.,0.));
#14868=DIRECTION('center_axis',(0.,0.,1.));
#14869=DIRECTION('ref_axis',(1.,0.,0.));
#14870=DIRECTION('center_axis',(0.,0.,1.));
#14871=DIRECTION('ref_axis',(1.,0.,0.));
#14872=DIRECTION('',(0.,0.,-1.));
#14873=DIRECTION('center_axis',(0.,0.,1.));
#14874=DIRECTION('ref_axis',(1.,0.,0.));
#14875=DIRECTION('center_axis',(0.,0.,-1.));
#14876=DIRECTION('ref_axis',(-1.,0.,0.));
#14877=DIRECTION('center_axis',(0.,0.,1.));
#14878=DIRECTION('ref_axis',(1.,0.,0.));
#14879=DIRECTION('center_axis',(0.,0.,1.));
#14880=DIRECTION('ref_axis',(1.,0.,0.));
#14881=DIRECTION('center_axis',(0.,0.,1.));
#14882=DIRECTION('ref_axis',(1.,0.,0.));
#14883=DIRECTION('',(0.,0.,-1.));
#14884=DIRECTION('center_axis',(0.,0.,1.));
#14885=DIRECTION('ref_axis',(1.,0.,0.));
#14886=DIRECTION('axis',(0.,0.,1.));
#14887=DIRECTION('refdir',(1.,0.,0.));
#14888=DIRECTION('center_axis',(0.,-0.70710678118654,-0.707106781186555));
#14889=DIRECTION('ref_axis',(-1.,0.,0.));
#14890=DIRECTION('',(0.,-0.707106781186555,0.70710678118654));
#14891=DIRECTION('',(-1.,0.,0.));
#14892=DIRECTION('center_axis',(0.,0.70710678118654,0.707106781186555));
#14893=DIRECTION('ref_axis',(0.,0.707106781186555,-0.70710678118654));
#14894=DIRECTION('',(1.,0.,0.));
#14895=DIRECTION('center_axis',(0.,1.,0.));
#14896=DIRECTION('ref_axis',(-1.,0.,0.));
#14897=DIRECTION('',(0.,0.,1.));
#14898=DIRECTION('',(1.,0.,0.));
#14899=DIRECTION('',(0.,0.,1.));
#14900=DIRECTION('center_axis',(1.,0.,0.));
#14901=DIRECTION('ref_axis',(0.,1.,0.));
#14902=DIRECTION('',(0.,1.,0.));
#14903=DIRECTION('',(0.,0.,1.));
#14904=DIRECTION('',(0.,1.,0.));
#14905=DIRECTION('',(0.,0.707106781186555,0.70710678118654));
#14906=DIRECTION('center_axis',(0.,0.70710678118654,-0.707106781186555));
#14907=DIRECTION('ref_axis',(-1.,0.,0.));
#14908=DIRECTION('',(0.,-0.707106781186555,-0.70710678118654));
#14909=DIRECTION('',(-1.,0.,0.));
#14910=DIRECTION('center_axis',(0.,-0.70710678118654,0.707106781186555));
#14911=DIRECTION('ref_axis',(0.,0.707106781186555,0.70710678118654));
#14912=DIRECTION('',(1.,0.,0.));
#14913=DIRECTION('center_axis',(0.,-1.,0.));
#14914=DIRECTION('ref_axis',(1.,0.,0.));
#14915=DIRECTION('',(0.,0.,-1.));
#14916=DIRECTION('',(-1.,0.,0.));
#14917=DIRECTION('',(0.,0.,1.));
#14918=DIRECTION('center_axis',(0.,0.,1.));
#14919=DIRECTION('ref_axis',(-1.,1.22464679914735E-16,0.));
#14920=DIRECTION('center_axis',(0.,0.70710678118654,-0.707106781186555));
#14921=DIRECTION('ref_axis',(0.,0.707106781186555,0.70710678118654));
#14922=DIRECTION('center_axis',(0.,0.,-1.));
#14923=DIRECTION('ref_axis',(1.,0.,0.));
#14924=DIRECTION('center_axis',(0.,-0.70710678118654,-0.707106781186555));
#14925=DIRECTION('ref_axis',(0.,0.707106781186555,-0.70710678118654));
#14926=DIRECTION('center_axis',(0.,0.,-1.));
#14927=DIRECTION('ref_axis',(1.,0.,0.));
#14928=DIRECTION('center_axis',(0.,-0.70710678118654,0.707106781186555));
#14929=DIRECTION('ref_axis',(1.,0.,0.));
#14930=DIRECTION('',(-1.,0.,0.));
#14931=DIRECTION('center_axis',(0.,0.,1.));
#14932=DIRECTION('ref_axis',(1.,0.,0.));
#14933=DIRECTION('',(-1.,0.,0.));
#14934=DIRECTION('',(0.,-1.,0.));
#14935=DIRECTION('center_axis',(0.,0.,1.));
#14936=DIRECTION('ref_axis',(1.,0.,0.));
#14937=DIRECTION('',(0.,-1.,0.));
#14938=DIRECTION('',(1.,0.,0.));
#14939=DIRECTION('',(0.,1.,0.));
#14940=DIRECTION('',(1.,0.,0.));
#14941=DIRECTION('center_axis',(0.,0.,-1.));
#14942=DIRECTION('ref_axis',(1.,0.,0.));
#14943=DIRECTION('center_axis',(0.,0.,-1.));
#14944=DIRECTION('ref_axis',(1.,0.,0.));
#14945=DIRECTION('center_axis',(0.,0.70710678118654,0.707106781186555));
#14946=DIRECTION('ref_axis',(1.,0.,0.));
#14947=DIRECTION('',(0.,0.707106781186555,-0.70710678118654));
#14948=DIRECTION('center_axis',(1.,0.,0.));
#14949=DIRECTION('ref_axis',(0.,1.,0.));
#14950=DIRECTION('',(0.,0.,1.));
#14951=DIRECTION('',(0.,-1.,0.));
#14952=DIRECTION('center_axis',(0.,0.,1.));
#14953=DIRECTION('ref_axis',(1.,0.,0.));
#14954=DIRECTION('center_axis',(0.,0.,1.));
#14955=DIRECTION('ref_axis',(1.,0.,0.));
#14956=DIRECTION('',(0.,0.,1.));
#14957=DIRECTION('center_axis',(0.,0.,1.));
#14958=DIRECTION('ref_axis',(1.,0.,0.));
#14959=DIRECTION('center_axis',(0.,0.,1.));
#14960=DIRECTION('ref_axis',(1.,0.,0.));
#14961=DIRECTION('',(0.,0.,1.));
#14962=DIRECTION('center_axis',(-1.,0.,0.));
#14963=DIRECTION('ref_axis',(0.,-1.,0.));
#14964=DIRECTION('',(0.,0.,1.));
#14965=DIRECTION('',(0.,1.,0.));
#14966=DIRECTION('',(0.,0.,1.));
#14967=DIRECTION('center_axis',(0.,-1.,0.));
#14968=DIRECTION('ref_axis',(1.,0.,0.));
#14969=DIRECTION('',(-1.,0.,0.));
#14970=DIRECTION('center_axis',(-1.,0.,0.));
#14971=DIRECTION('ref_axis',(0.,-1.,0.));
#14972=DIRECTION('',(0.,0.,-1.));
#14973=DIRECTION('',(0.,0.,1.));
#14974=DIRECTION('',(0.,-1.,0.));
#14975=DIRECTION('center_axis',(0.,1.,0.));
#14976=DIRECTION('ref_axis',(-1.,0.,0.));
#14977=DIRECTION('',(-1.,0.,0.));
#14978=DIRECTION('center_axis',(0.,0.,1.));
#14979=DIRECTION('ref_axis',(1.,0.,0.));
#14980=DIRECTION('center_axis',(0.,0.,1.));
#14981=DIRECTION('ref_axis',(1.,0.,0.));
#14982=DIRECTION('center_axis',(0.,0.,1.));
#14983=DIRECTION('ref_axis',(-1.,-1.22464679914735E-16,0.));
#14984=DIRECTION('axis',(0.,0.,1.));
#14985=DIRECTION('refdir',(1.,0.,0.));
#14986=DIRECTION('center_axis',(-1.,0.,0.));
#14987=DIRECTION('ref_axis',(0.,0.,1.));
#14988=DIRECTION('',(1.,0.,0.));
#14989=DIRECTION('center_axis',(-1.,0.,0.));
#14990=DIRECTION('ref_axis',(0.,0.,1.));
#14991=DIRECTION('center_axis',(-1.,0.,0.));
#14992=DIRECTION('ref_axis',(0.,0.,1.));
#14993=DIRECTION('',(1.,0.,0.));
#14994=DIRECTION('center_axis',(-1.,0.,0.));
#14995=DIRECTION('ref_axis',(0.,0.,1.));
#14996=DIRECTION('',(1.,0.,0.));
#14997=DIRECTION('center_axis',(-1.,0.,0.));
#14998=DIRECTION('ref_axis',(0.,0.,1.));
#14999=DIRECTION('',(1.,0.,0.));
#15000=DIRECTION('center_axis',(-1.,0.,0.));
#15001=DIRECTION('ref_axis',(0.,0.,1.));
#15002=DIRECTION('',(1.,0.,0.));
#15003=DIRECTION('center_axis',(-1.,0.,0.));
#15004=DIRECTION('ref_axis',(0.,0.,1.));
#15005=DIRECTION('',(1.,0.,0.));
#15006=DIRECTION('center_axis',(-1.,0.,0.));
#15007=DIRECTION('ref_axis',(0.,-0.376634011382756,-0.92636214380216));
#15008=DIRECTION('',(-1.,0.,0.));
#15009=DIRECTION('center_axis',(-1.,0.,0.));
#15010=DIRECTION('ref_axis',(0.,1.36963031528353E-14,1.));
#15011=DIRECTION('center_axis',(-1.,0.,0.));
#15012=DIRECTION('ref_axis',(0.,1.36963031528353E-14,1.));
#15013=DIRECTION('',(-1.,0.,0.));
#15014=DIRECTION('center_axis',(-1.,0.,0.));
#15015=DIRECTION('ref_axis',(0.,1.36963031528353E-14,1.));
#15016=DIRECTION('center_axis',(-1.,0.,0.));
#15017=DIRECTION('ref_axis',(0.,1.36963031528353E-14,1.));
#15018=DIRECTION('',(-1.,0.,0.));
#15019=DIRECTION('center_axis',(-1.,0.,0.));
#15020=DIRECTION('ref_axis',(0.,1.36963031528353E-14,1.));
#15021=DIRECTION('',(-1.,0.,0.));
#15022=DIRECTION('center_axis',(-1.,0.,0.));
#15023=DIRECTION('ref_axis',(0.,1.36963031528353E-14,1.));
#15024=DIRECTION('',(-1.,0.,0.));
#15025=DIRECTION('center_axis',(-1.,0.,0.));
#15026=DIRECTION('ref_axis',(0.,1.36963031528353E-14,1.));
#15027=DIRECTION('',(-1.,0.,0.));
#15028=DIRECTION('center_axis',(1.,0.,0.));
#15029=DIRECTION('ref_axis',(0.,0.,-1.));
#15030=DIRECTION('center_axis',(1.,0.,0.));
#15031=DIRECTION('ref_axis',(0.,0.,1.));
#15032=DIRECTION('center_axis',(1.,0.,0.));
#15033=DIRECTION('ref_axis',(0.,0.,1.));
#15034=DIRECTION('center_axis',(1.,0.,0.));
#15035=DIRECTION('ref_axis',(0.,0.,-1.));
#15036=DIRECTION('center_axis',(-1.,0.,0.));
#15037=DIRECTION('ref_axis',(0.,0.,1.));
#15038=DIRECTION('center_axis',(-1.,0.,0.));
#15039=DIRECTION('ref_axis',(0.,0.,1.));
#15040=DIRECTION('center_axis',(1.,0.,0.));
#15041=DIRECTION('ref_axis',(0.,1.36963031528353E-14,1.));
#15042=DIRECTION('center_axis',(-1.,0.,0.));
#15043=DIRECTION('ref_axis',(0.,0.457593006249823,0.88916176291564));
#15044=DIRECTION('center_axis',(0.,0.866025403784439,0.5));
#15045=DIRECTION('ref_axis',(0.,0.5,-0.866025403784439));
#15046=DIRECTION('',(0.,0.5,-0.866025403784439));
#15047=DIRECTION('',(-1.,0.,0.));
#15048=DIRECTION('',(0.,0.5,-0.866025403784439));
#15049=DIRECTION('',(-1.,0.,0.));
#15050=DIRECTION('center_axis',(0.,0.,1.));
#15051=DIRECTION('ref_axis',(0.,1.,0.));
#15052=DIRECTION('',(0.,1.,0.));
#15053=DIRECTION('',(-1.,0.,0.));
#15054=DIRECTION('',(0.,1.,0.));
#15055=DIRECTION('center_axis',(0.,-0.866025403784439,0.5));
#15056=DIRECTION('ref_axis',(0.,0.5,0.866025403784439));
#15057=DIRECTION('',(0.,0.5,0.866025403784439));
#15058=DIRECTION('',(-1.,0.,0.));
#15059=DIRECTION('',(0.,0.5,0.866025403784439));
#15060=DIRECTION('center_axis',(0.,-0.866025403784439,-0.499999999999999));
#15061=DIRECTION('ref_axis',(0.,-0.499999999999999,0.866025403784439));
#15062=DIRECTION('',(0.,-0.499999999999999,0.866025403784439));
#15063=DIRECTION('',(-1.,0.,0.));
#15064=DIRECTION('',(0.,-0.499999999999999,0.866025403784439));
#15065=DIRECTION('center_axis',(0.,0.,-1.));
#15066=DIRECTION('ref_axis',(0.,-1.,0.));
#15067=DIRECTION('',(0.,-1.,0.));
#15068=DIRECTION('',(-1.,0.,0.));
#15069=DIRECTION('',(0.,-1.,0.));
#15070=DIRECTION('center_axis',(0.,0.866025403784439,-0.5));
#15071=DIRECTION('ref_axis',(0.,-0.5,-0.866025403784439));
#15072=DIRECTION('',(0.,-0.5,-0.866025403784439));
#15073=DIRECTION('',(0.,-0.5,-0.866025403784439));
#15074=DIRECTION('center_axis',(-1.,0.,0.));
#15075=DIRECTION('ref_axis',(0.,0.,1.));
#15076=DIRECTION('center_axis',(1.,0.,0.));
#15077=DIRECTION('ref_axis',(0.,0.,-1.));
#15078=DIRECTION('center_axis',(-1.,0.,0.));
#15079=DIRECTION('ref_axis',(0.,0.,1.));
#15080=DIRECTION('center_axis',(-1.,0.,0.));
#15081=DIRECTION('ref_axis',(0.,0.,1.));
#15082=DIRECTION('',(0.70710678118655,8.6595605623549E-17,0.707106781186545));
#15083=DIRECTION('center_axis',(-1.,0.,0.));
#15084=DIRECTION('ref_axis',(0.,-0.953985326168334,0.299853293221031));
#15085=DIRECTION('center_axis',(1.,0.,0.));
#15086=DIRECTION('ref_axis',(0.,0.,1.));
#15087=DIRECTION('center_axis',(1.,0.,0.));
#15088=DIRECTION('ref_axis',(0.,0.,1.));
#15089=DIRECTION('center_axis',(-1.,0.,0.));
#15090=DIRECTION('ref_axis',(0.,0.,1.));
#15091=DIRECTION('',(0.707106781186549,-8.65956056235492E-17,-0.707106781186546));
#15092=DIRECTION('center_axis',(-1.,0.,0.));
#15093=DIRECTION('ref_axis',(0.,0.,1.));
#15094=DIRECTION('axis',(0.,0.,1.));
#15095=DIRECTION('refdir',(1.,0.,0.));
#15096=DIRECTION('center_axis',(0.,0.,1.));
#15097=DIRECTION('ref_axis',(1.,0.,0.));
#15098=DIRECTION('',(0.,0.,-1.));
#15099=DIRECTION('center_axis',(0.,0.,1.));
#15100=DIRECTION('ref_axis',(1.,0.,0.));
#15101=DIRECTION('center_axis',(0.,0.,1.));
#15102=DIRECTION('ref_axis',(1.,0.,0.));
#15103=DIRECTION('',(0.,0.,-1.));
#15104=DIRECTION('center_axis',(0.,0.,1.));
#15105=DIRECTION('ref_axis',(1.,0.,0.));
#15106=DIRECTION('',(0.,0.,-1.));
#15107=DIRECTION('center_axis',(0.,0.,1.));
#15108=DIRECTION('ref_axis',(1.,0.,0.));
#15109=DIRECTION('',(0.,0.,-1.));
#15110=DIRECTION('center_axis',(0.,0.,1.));
#15111=DIRECTION('ref_axis',(1.,0.,0.));
#15112=DIRECTION('',(0.,0.,-1.));
#15113=DIRECTION('center_axis',(0.,0.,1.));
#15114=DIRECTION('ref_axis',(1.,0.,0.));
#15115=DIRECTION('',(0.,0.,-1.));
#15116=DIRECTION('center_axis',(0.,0.,1.));
#15117=DIRECTION('ref_axis',(1.,0.,0.));
#15118=DIRECTION('',(0.,0.,-1.));
#15119=DIRECTION('center_axis',(0.,0.,1.));
#15120=DIRECTION('ref_axis',(1.,0.,0.));
#15121=DIRECTION('',(0.,0.,-1.));
#15122=DIRECTION('center_axis',(0.,0.,1.));
#15123=DIRECTION('ref_axis',(1.,0.,0.));
#15124=DIRECTION('',(0.,0.,-1.));
#15125=DIRECTION('center_axis',(0.,0.,1.));
#15126=DIRECTION('ref_axis',(1.,0.,0.));
#15127=DIRECTION('',(0.,0.,-1.));
#15128=DIRECTION('center_axis',(0.,0.,1.));
#15129=DIRECTION('ref_axis',(1.,0.,0.));
#15130=DIRECTION('',(0.,0.,-1.));
#15131=DIRECTION('center_axis',(0.,0.,1.));
#15132=DIRECTION('ref_axis',(1.,0.,0.));
#15133=DIRECTION('',(0.,0.,-1.));
#15134=DIRECTION('center_axis',(0.,0.,1.));
#15135=DIRECTION('ref_axis',(1.,0.,0.));
#15136=DIRECTION('',(0.,0.,-1.));
#15137=DIRECTION('center_axis',(0.,0.,1.));
#15138=DIRECTION('ref_axis',(1.,0.,0.));
#15139=DIRECTION('',(0.,0.,-1.));
#15140=DIRECTION('center_axis',(0.,0.,1.));
#15141=DIRECTION('ref_axis',(1.,0.,0.));
#15142=DIRECTION('',(0.,0.,-1.));
#15143=DIRECTION('center_axis',(0.,0.,1.));
#15144=DIRECTION('ref_axis',(1.,0.,0.));
#15145=DIRECTION('',(0.,0.,-1.));
#15146=DIRECTION('center_axis',(0.,0.,1.));
#15147=DIRECTION('ref_axis',(1.,0.,0.));
#15148=DIRECTION('',(0.,0.,-1.));
#15149=DIRECTION('center_axis',(0.,0.,1.));
#15150=DIRECTION('ref_axis',(1.,0.,0.));
#15151=DIRECTION('',(0.,0.,-1.));
#15152=DIRECTION('center_axis',(0.,0.,1.));
#15153=DIRECTION('ref_axis',(1.,0.,0.));
#15154=DIRECTION('',(0.,0.,-1.));
#15155=DIRECTION('center_axis',(0.,0.,1.));
#15156=DIRECTION('ref_axis',(1.,0.,0.));
#15157=DIRECTION('',(0.,0.,-1.));
#15158=DIRECTION('center_axis',(0.,0.,1.));
#15159=DIRECTION('ref_axis',(1.,0.,0.));
#15160=DIRECTION('',(0.,0.,-1.));
#15161=DIRECTION('center_axis',(0.,0.,1.));
#15162=DIRECTION('ref_axis',(1.,0.,0.));
#15163=DIRECTION('',(0.,0.,-1.));
#15164=DIRECTION('center_axis',(0.,0.,1.));
#15165=DIRECTION('ref_axis',(1.,0.,0.));
#15166=DIRECTION('',(0.,0.,-1.));
#15167=DIRECTION('center_axis',(0.,0.,1.));
#15168=DIRECTION('ref_axis',(1.,0.,0.));
#15169=DIRECTION('',(0.,0.,-1.));
#15170=DIRECTION('center_axis',(0.,0.,1.));
#15171=DIRECTION('ref_axis',(1.,-8.50999688392278E-15,0.));
#15172=DIRECTION('',(0.,0.,1.));
#15173=DIRECTION('center_axis',(0.,0.,1.));
#15174=DIRECTION('ref_axis',(1.,-8.50999688392278E-15,0.));
#15175=DIRECTION('center_axis',(0.,0.,1.));
#15176=DIRECTION('ref_axis',(1.,-8.50999688392278E-15,0.));
#15177=DIRECTION('',(0.,0.,1.));
#15178=DIRECTION('center_axis',(0.,0.,1.));
#15179=DIRECTION('ref_axis',(1.,-8.50999688392278E-15,0.));
#15180=DIRECTION('center_axis',(0.,0.,1.));
#15181=DIRECTION('ref_axis',(1.,-8.50999688392278E-15,0.));
#15182=DIRECTION('',(0.,0.,1.));
#15183=DIRECTION('center_axis',(0.,0.,1.));
#15184=DIRECTION('ref_axis',(1.,-8.50999688392278E-15,0.));
#15185=DIRECTION('',(0.,0.,1.));
#15186=DIRECTION('center_axis',(0.,0.,1.));
#15187=DIRECTION('ref_axis',(1.,-8.50999688392278E-15,0.));
#15188=DIRECTION('',(0.,0.,1.));
#15189=DIRECTION('center_axis',(0.,0.,1.));
#15190=DIRECTION('ref_axis',(1.,-8.50999688392278E-15,0.));
#15191=DIRECTION('',(0.,0.,1.));
#15192=DIRECTION('center_axis',(0.,0.,1.));
#15193=DIRECTION('ref_axis',(1.,-8.50999688392278E-15,0.));
#15194=DIRECTION('',(0.,0.,1.));
#15195=DIRECTION('center_axis',(0.,0.,1.));
#15196=DIRECTION('ref_axis',(1.,-8.50999688392278E-15,0.));
#15197=DIRECTION('',(0.,0.,1.));
#15198=DIRECTION('center_axis',(0.,0.,1.));
#15199=DIRECTION('ref_axis',(1.,-8.50999688392278E-15,0.));
#15200=DIRECTION('',(0.,0.,1.));
#15201=DIRECTION('center_axis',(0.,0.,1.));
#15202=DIRECTION('ref_axis',(1.,-8.50999688392278E-15,0.));
#15203=DIRECTION('',(0.,0.,1.));
#15204=DIRECTION('center_axis',(0.,0.,1.));
#15205=DIRECTION('ref_axis',(1.,-8.50999688392278E-15,0.));
#15206=DIRECTION('',(0.,0.,1.));
#15207=DIRECTION('center_axis',(0.,0.,1.));
#15208=DIRECTION('ref_axis',(1.,-8.50999688392278E-15,0.));
#15209=DIRECTION('',(0.,0.,1.));
#15210=DIRECTION('center_axis',(0.,0.,1.));
#15211=DIRECTION('ref_axis',(1.,-8.50999688392278E-15,0.));
#15212=DIRECTION('',(0.,0.,1.));
#15213=DIRECTION('center_axis',(0.,0.,1.));
#15214=DIRECTION('ref_axis',(1.,-8.50999688392278E-15,0.));
#15215=DIRECTION('',(0.,0.,1.));
#15216=DIRECTION('center_axis',(0.,0.,1.));
#15217=DIRECTION('ref_axis',(1.,-8.50999688392278E-15,0.));
#15218=DIRECTION('',(0.,0.,1.));
#15219=DIRECTION('center_axis',(0.,0.,1.));
#15220=DIRECTION('ref_axis',(1.,-8.50999688392278E-15,0.));
#15221=DIRECTION('',(0.,0.,1.));
#15222=DIRECTION('center_axis',(0.,0.,1.));
#15223=DIRECTION('ref_axis',(1.,-8.50999688392278E-15,0.));
#15224=DIRECTION('',(0.,0.,1.));
#15225=DIRECTION('center_axis',(0.,0.,1.));
#15226=DIRECTION('ref_axis',(1.,-8.50999688392278E-15,0.));
#15227=DIRECTION('',(0.,0.,1.));
#15228=DIRECTION('center_axis',(0.,0.,1.));
#15229=DIRECTION('ref_axis',(1.,-8.50999688392278E-15,0.));
#15230=DIRECTION('',(0.,0.,1.));
#15231=DIRECTION('center_axis',(0.,0.,1.));
#15232=DIRECTION('ref_axis',(1.,-8.50999688392278E-15,0.));
#15233=DIRECTION('',(0.,0.,1.));
#15234=DIRECTION('center_axis',(0.,0.,1.));
#15235=DIRECTION('ref_axis',(1.,-8.50999688392278E-15,0.));
#15236=DIRECTION('',(0.,0.,1.));
#15237=DIRECTION('center_axis',(0.,0.,1.));
#15238=DIRECTION('ref_axis',(1.,-8.50999688392278E-15,0.));
#15239=DIRECTION('',(0.,0.,1.));
#15240=DIRECTION('center_axis',(0.,0.,1.));
#15241=DIRECTION('ref_axis',(1.,-8.50999688392278E-15,0.));
#15242=DIRECTION('',(0.,0.,1.));
#15243=DIRECTION('center_axis',(0.,0.,1.));
#15244=DIRECTION('ref_axis',(1.,-8.50999688392278E-15,0.));
#15245=DIRECTION('',(0.,0.,1.));
#15246=DIRECTION('center_axis',(0.,0.,1.));
#15247=DIRECTION('ref_axis',(1.,0.,0.));
#15248=DIRECTION('center_axis',(0.,0.,1.));
#15249=DIRECTION('ref_axis',(1.,0.,0.));
#15250=DIRECTION('center_axis',(0.,0.,1.));
#15251=DIRECTION('ref_axis',(1.,0.,0.));
#15252=DIRECTION('center_axis',(0.,0.,-1.));
#15253=DIRECTION('ref_axis',(1.,-8.50999688392278E-15,0.));
#15254=DIRECTION('center_axis',(0.,0.,1.));
#15255=DIRECTION('ref_axis',(1.,-8.50999688392278E-15,0.));
#15256=DIRECTION('center_axis',(0.,0.,1.));
#15257=DIRECTION('ref_axis',(1.,0.,0.));
#15258=DIRECTION('',(-0.857492925712544,-1.05012596676537E-16,0.514495755427526));
#15259=DIRECTION('center_axis',(0.,0.,-1.));
#15260=DIRECTION('ref_axis',(1.,0.,0.));
#15261=DIRECTION('center_axis',(0.866025403784439,0.5,0.));
#15262=DIRECTION('ref_axis',(0.5,-0.866025403784439,0.));
#15263=DIRECTION('',(0.5,-0.866025403784439,0.));
#15264=DIRECTION('',(0.,0.,-1.));
#15265=DIRECTION('',(0.5,-0.866025403784439,0.));
#15266=DIRECTION('',(0.,0.,-1.));
#15267=DIRECTION('center_axis',(1.92296268638356E-16,1.,0.));
#15268=DIRECTION('ref_axis',(1.,-1.92296268638356E-16,0.));
#15269=DIRECTION('',(1.,-1.92296268638356E-16,0.));
#15270=DIRECTION('',(0.,0.,-1.));
#15271=DIRECTION('',(1.,-1.92296268638356E-16,0.));
#15272=DIRECTION('center_axis',(-0.866025403784438,0.5,0.));
#15273=DIRECTION('ref_axis',(0.5,0.866025403784438,0.));
#15274=DIRECTION('',(0.5,0.866025403784438,0.));
#15275=DIRECTION('',(0.,0.,-1.));
#15276=DIRECTION('',(0.5,0.866025403784438,0.));
#15277=DIRECTION('center_axis',(-0.866025403784439,-0.5,0.));
#15278=DIRECTION('ref_axis',(-0.5,0.866025403784439,0.));
#15279=DIRECTION('',(-0.5,0.866025403784439,0.));
#15280=DIRECTION('',(0.,0.,-1.));
#15281=DIRECTION('',(-0.5,0.866025403784439,0.));
#15282=DIRECTION('center_axis',(-1.92296268638356E-16,-1.,0.));
#15283=DIRECTION('ref_axis',(-1.,1.92296268638356E-16,0.));
#15284=DIRECTION('',(-1.,1.92296268638356E-16,0.));
#15285=DIRECTION('',(0.,0.,-1.));
#15286=DIRECTION('',(-1.,1.92296268638356E-16,0.));
#15287=DIRECTION('center_axis',(0.866025403784439,-0.5,0.));
#15288=DIRECTION('ref_axis',(-0.5,-0.866025403784439,0.));
#15289=DIRECTION('',(-0.5,-0.866025403784439,0.));
#15290=DIRECTION('',(-0.5,-0.866025403784439,0.));
#15291=DIRECTION('center_axis',(0.,0.,-1.));
#15292=DIRECTION('ref_axis',(-1.,0.,0.));
#15293=DIRECTION('center_axis',(-0.713210659190727,-0.700949752561999,0.));
#15294=DIRECTION('ref_axis',(-0.700949752561999,0.713210659190727,0.));
#15295=DIRECTION('',(0.,0.,1.));
#15296=DIRECTION('',(-0.700949752561999,0.713210659190727,0.));
#15297=DIRECTION('',(0.,0.,-1.));
#15298=DIRECTION('',(-0.700949752561999,0.713210659190727,0.));
#15299=DIRECTION('center_axis',(0.,0.,1.));
#15300=DIRECTION('ref_axis',(1.,0.,0.));
#15301=DIRECTION('center_axis',(0.,0.,1.));
#15302=DIRECTION('ref_axis',(1.,0.,0.));
#15303=DIRECTION('',(0.995401637679912,0.0957892462865752,0.));
#15304=DIRECTION('center_axis',(-0.0957892462865752,0.995401637679912,0.));
#15305=DIRECTION('ref_axis',(0.995401637679912,0.0957892462865752,0.));
#15306=DIRECTION('',(0.,0.,-1.));
#15307=DIRECTION('',(0.995401637679912,0.0957892462865752,0.));
#15308=DIRECTION('center_axis',(0.,0.,-1.));
#15309=DIRECTION('ref_axis',(-1.,0.,0.));
#15310=DIRECTION('center_axis',(0.,0.,-1.));
#15311=DIRECTION('ref_axis',(1.,0.,0.));
#15312=DIRECTION('center_axis',(-0.909937728342724,-0.414744898146418,0.));
#15313=DIRECTION('ref_axis',(-0.414744898146418,0.909937728342724,0.));
#15314=DIRECTION('',(0.,0.,1.));
#15315=DIRECTION('',(-0.414744898146418,0.909937728342724,0.));
#15316=DIRECTION('',(0.,0.,-1.));
#15317=DIRECTION('',(-0.414744898146418,0.909937728342724,0.));
#15318=DIRECTION('center_axis',(0.,0.,1.));
#15319=DIRECTION('ref_axis',(1.,0.,0.));
#15320=DIRECTION('center_axis',(0.,0.,1.));
#15321=DIRECTION('ref_axis',(1.,0.,0.));
#15322=DIRECTION('',(0.968133425390015,-0.250434962899744,0.));
#15323=DIRECTION('center_axis',(0.250434962899744,0.968133425390015,0.));
#15324=DIRECTION('ref_axis',(0.968133425390015,-0.250434962899744,0.));
#15325=DIRECTION('',(0.,0.,-1.));
#15326=DIRECTION('',(0.968133425390015,-0.250434962899744,0.));
#15327=DIRECTION('center_axis',(0.,0.,-1.));
#15328=DIRECTION('ref_axis',(-1.,0.,0.));
#15329=DIRECTION('center_axis',(0.,0.,-1.));
#15330=DIRECTION('ref_axis',(1.,0.,0.));
#15331=DIRECTION('center_axis',(-0.996912878205979,-0.0785156880315736,
0.));
#15332=DIRECTION('ref_axis',(-0.0785156880315736,0.996912878205979,0.));
#15333=DIRECTION('',(0.,0.,1.));
#15334=DIRECTION('',(-0.0785156880315736,0.996912878205979,0.));
#15335=DIRECTION('',(0.,0.,-1.));
#15336=DIRECTION('',(-0.0785156880315736,0.996912878205979,0.));
#15337=DIRECTION('center_axis',(0.,0.,1.));
#15338=DIRECTION('ref_axis',(1.,0.,0.));
#15339=DIRECTION('center_axis',(0.,0.,1.));
#15340=DIRECTION('ref_axis',(1.,0.,0.));
#15341=DIRECTION('',(0.824094033870449,-0.566453019533952,0.));
#15342=DIRECTION('center_axis',(0.566453019533952,0.824094033870449,0.));
#15343=DIRECTION('ref_axis',(0.824094033870449,-0.566453019533952,0.));
#15344=DIRECTION('',(0.,0.,-1.));
#15345=DIRECTION('',(0.824094033870449,-0.566453019533952,0.));
#15346=DIRECTION('center_axis',(0.,0.,-1.));
#15347=DIRECTION('ref_axis',(-1.,0.,0.));
#15348=DIRECTION('center_axis',(0.,0.,-1.));
#15349=DIRECTION('ref_axis',(1.,0.,0.));
#15350=DIRECTION('center_axis',(-0.963645622090473,0.26718367282801,0.));
#15351=DIRECTION('ref_axis',(0.26718367282801,0.963645622090473,0.));
#15352=DIRECTION('',(0.,0.,1.));
#15353=DIRECTION('',(0.26718367282801,0.963645622090473,0.));
#15354=DIRECTION('',(0.,0.,-1.));
#15355=DIRECTION('',(0.26718367282801,0.963645622090473,0.));
#15356=DIRECTION('center_axis',(0.,0.,1.));
#15357=DIRECTION('ref_axis',(1.,0.,0.));
#15358=DIRECTION('center_axis',(0.,0.,1.));
#15359=DIRECTION('ref_axis',(1.,0.,0.));
#15360=DIRECTION('',(0.580656739533499,-0.814148482056146,0.));
#15361=DIRECTION('center_axis',(0.814148482056146,0.580656739533499,0.));
#15362=DIRECTION('ref_axis',(0.580656739533499,-0.814148482056146,0.));
#15363=DIRECTION('',(0.,0.,-1.));
#15364=DIRECTION('',(0.580656739533499,-0.814148482056146,0.));
#15365=DIRECTION('center_axis',(0.,0.,-1.));
#15366=DIRECTION('ref_axis',(-1.,0.,0.));
#15367=DIRECTION('center_axis',(0.,0.,-1.));
#15368=DIRECTION('ref_axis',(1.,0.,0.));
#15369=DIRECTION('center_axis',(-0.814148482056146,0.580656739533499,0.));
#15370=DIRECTION('ref_axis',(0.580656739533499,0.814148482056146,0.));
#15371=DIRECTION('',(0.,0.,1.));
#15372=DIRECTION('',(0.580656739533499,0.814148482056146,0.));
#15373=DIRECTION('',(0.,0.,-1.));
#15374=DIRECTION('',(0.580656739533499,0.814148482056146,0.));
#15375=DIRECTION('center_axis',(0.,0.,1.));
#15376=DIRECTION('ref_axis',(1.,0.,0.));
#15377=DIRECTION('center_axis',(0.,0.,1.));
#15378=DIRECTION('ref_axis',(1.,0.,0.));
#15379=DIRECTION('',(0.267183672828016,-0.963645622090472,0.));
#15380=DIRECTION('center_axis',(0.963645622090472,0.267183672828016,0.));
#15381=DIRECTION('ref_axis',(0.267183672828016,-0.963645622090472,0.));
#15382=DIRECTION('',(0.,0.,-1.));
#15383=DIRECTION('',(0.267183672828016,-0.963645622090472,0.));
#15384=DIRECTION('center_axis',(0.,0.,-1.));
#15385=DIRECTION('ref_axis',(-1.,0.,0.));
#15386=DIRECTION('center_axis',(0.,0.,-1.));
#15387=DIRECTION('ref_axis',(1.,0.,0.));
#15388=DIRECTION('center_axis',(-0.56645301953395,0.82409403387045,0.));
#15389=DIRECTION('ref_axis',(0.82409403387045,0.56645301953395,0.));
#15390=DIRECTION('',(0.,0.,1.));
#15391=DIRECTION('',(0.82409403387045,0.56645301953395,0.));
#15392=DIRECTION('',(0.,0.,-1.));
#15393=DIRECTION('',(0.82409403387045,0.56645301953395,0.));
#15394=DIRECTION('center_axis',(0.,0.,1.));
#15395=DIRECTION('ref_axis',(1.,0.,0.));
#15396=DIRECTION('center_axis',(0.,0.,1.));
#15397=DIRECTION('ref_axis',(1.,0.,0.));
#15398=DIRECTION('',(-0.0785156880315734,-0.996912878205979,0.));
#15399=DIRECTION('center_axis',(0.996912878205979,-0.0785156880315734,0.));
#15400=DIRECTION('ref_axis',(-0.0785156880315734,-0.996912878205979,0.));
#15401=DIRECTION('',(0.,0.,-1.));
#15402=DIRECTION('',(-0.0785156880315734,-0.996912878205979,0.));
#15403=DIRECTION('center_axis',(0.,0.,-1.));
#15404=DIRECTION('ref_axis',(-1.,0.,0.));
#15405=DIRECTION('center_axis',(0.,0.,-1.));
#15406=DIRECTION('ref_axis',(1.,0.,0.));
#15407=DIRECTION('center_axis',(-0.250434962899748,0.968133425390014,0.));
#15408=DIRECTION('ref_axis',(0.968133425390014,0.250434962899748,0.));
#15409=DIRECTION('',(0.,0.,1.));
#15410=DIRECTION('',(0.968133425390014,0.250434962899748,0.));
#15411=DIRECTION('',(0.,0.,-1.));
#15412=DIRECTION('',(0.968133425390014,0.250434962899748,0.));
#15413=DIRECTION('center_axis',(0.,0.,1.));
#15414=DIRECTION('ref_axis',(1.,0.,0.));
#15415=DIRECTION('center_axis',(0.,0.,1.));
#15416=DIRECTION('ref_axis',(1.,0.,0.));
#15417=DIRECTION('',(-0.414744898146415,-0.909937728342726,0.));
#15418=DIRECTION('center_axis',(0.909937728342726,-0.414744898146415,0.));
#15419=DIRECTION('ref_axis',(-0.414744898146415,-0.909937728342726,0.));
#15420=DIRECTION('',(0.,0.,-1.));
#15421=DIRECTION('',(-0.414744898146415,-0.909937728342726,0.));
#15422=DIRECTION('center_axis',(0.,0.,-1.));
#15423=DIRECTION('ref_axis',(-1.,0.,0.));
#15424=DIRECTION('center_axis',(0.,0.,-1.));
#15425=DIRECTION('ref_axis',(1.,0.,0.));
#15426=DIRECTION('center_axis',(0.0957892462865784,0.995401637679911,0.));
#15427=DIRECTION('ref_axis',(0.995401637679911,-0.0957892462865784,0.));
#15428=DIRECTION('',(0.,0.,1.));
#15429=DIRECTION('',(0.995401637679911,-0.0957892462865784,0.));
#15430=DIRECTION('',(0.,0.,-1.));
#15431=DIRECTION('',(0.995401637679911,-0.0957892462865784,0.));
#15432=DIRECTION('center_axis',(0.,0.,1.));
#15433=DIRECTION('ref_axis',(1.,0.,0.));
#15434=DIRECTION('center_axis',(0.,0.,1.));
#15435=DIRECTION('ref_axis',(1.,0.,0.));
#15436=DIRECTION('',(-0.700949752562001,-0.713210659190726,0.));
#15437=DIRECTION('center_axis',(0.713210659190726,-0.700949752562001,0.));
#15438=DIRECTION('ref_axis',(-0.700949752562001,-0.713210659190726,0.));
#15439=DIRECTION('',(0.,0.,-1.));
#15440=DIRECTION('',(-0.700949752562001,-0.713210659190726,0.));
#15441=DIRECTION('center_axis',(0.,0.,-1.));
#15442=DIRECTION('ref_axis',(-1.,0.,0.));
#15443=DIRECTION('center_axis',(0.,0.,-1.));
#15444=DIRECTION('ref_axis',(1.,0.,0.));
#15445=DIRECTION('center_axis',(0.43045985867203,0.902609721902028,0.));
#15446=DIRECTION('ref_axis',(0.902609721902028,-0.43045985867203,0.));
#15447=DIRECTION('',(0.,0.,1.));
#15448=DIRECTION('',(0.902609721902028,-0.43045985867203,0.));
#15449=DIRECTION('',(0.,0.,-1.));
#15450=DIRECTION('',(0.902609721902028,-0.43045985867203,0.));
#15451=DIRECTION('center_axis',(0.,0.,1.));
#15452=DIRECTION('ref_axis',(1.,0.,0.));
#15453=DIRECTION('center_axis',(0.,0.,1.));
#15454=DIRECTION('ref_axis',(1.,0.,0.));
#15455=DIRECTION('',(-0.902609721902028,-0.43045985867203,0.));
#15456=DIRECTION('center_axis',(0.,0.,1.));
#15457=DIRECTION('ref_axis',(1.,0.,0.));
#15458=DIRECTION('center_axis',(0.43045985867203,-0.902609721902028,0.));
#15459=DIRECTION('ref_axis',(-0.902609721902028,-0.43045985867203,0.));
#15460=DIRECTION('',(0.,0.,-1.));
#15461=DIRECTION('',(-0.902609721902028,-0.43045985867203,0.));
#15462=DIRECTION('center_axis',(0.,0.,-1.));
#15463=DIRECTION('ref_axis',(-1.,0.,0.));
#15464=DIRECTION('center_axis',(0.,0.,-1.));
#15465=DIRECTION('ref_axis',(1.,0.,0.));
#15466=DIRECTION('center_axis',(0.,0.,-1.));
#15467=DIRECTION('ref_axis',(1.,0.,0.));
#15468=DIRECTION('center_axis',(0.580656739533499,0.814148482056146,0.));
#15469=DIRECTION('ref_axis',(0.814148482056146,-0.580656739533499,0.));
#15470=DIRECTION('',(0.,0.,1.));
#15471=DIRECTION('',(0.814148482056146,-0.580656739533499,0.));
#15472=DIRECTION('',(0.,0.,-1.));
#15473=DIRECTION('',(0.814148482056146,-0.580656739533499,0.));
#15474=DIRECTION('center_axis',(0.,0.,1.));
#15475=DIRECTION('ref_axis',(1.,0.,0.));
#15476=DIRECTION('center_axis',(0.,0.,1.));
#15477=DIRECTION('ref_axis',(1.,0.,0.));
#15478=DIRECTION('',(-0.963645622090472,-0.267183672828013,0.));
#15479=DIRECTION('center_axis',(0.267183672828013,-0.963645622090472,0.));
#15480=DIRECTION('ref_axis',(-0.963645622090472,-0.267183672828013,0.));
#15481=DIRECTION('',(0.,0.,-1.));
#15482=DIRECTION('',(-0.963645622090472,-0.267183672828013,0.));
#15483=DIRECTION('center_axis',(0.,0.,-1.));
#15484=DIRECTION('ref_axis',(-1.,0.,0.));
#15485=DIRECTION('center_axis',(0.,0.,-1.));
#15486=DIRECTION('ref_axis',(1.,0.,0.));
#15487=DIRECTION('center_axis',(0.824094033870453,0.566453019533945,0.));
#15488=DIRECTION('ref_axis',(0.566453019533945,-0.824094033870453,0.));
#15489=DIRECTION('',(0.,0.,1.));
#15490=DIRECTION('',(0.566453019533945,-0.824094033870453,0.));
#15491=DIRECTION('',(0.,0.,-1.));
#15492=DIRECTION('',(0.566453019533945,-0.824094033870453,0.));
#15493=DIRECTION('center_axis',(0.,0.,1.));
#15494=DIRECTION('ref_axis',(1.,0.,0.));
#15495=DIRECTION('center_axis',(0.,0.,1.));
#15496=DIRECTION('ref_axis',(1.,0.,0.));
#15497=DIRECTION('',(-0.996912878205979,0.078515688031577,0.));
#15498=DIRECTION('center_axis',(-0.078515688031577,-0.996912878205979,0.));
#15499=DIRECTION('ref_axis',(-0.996912878205979,0.078515688031577,0.));
#15500=DIRECTION('',(0.,0.,-1.));
#15501=DIRECTION('',(-0.996912878205979,0.078515688031577,0.));
#15502=DIRECTION('center_axis',(0.,0.,-1.));
#15503=DIRECTION('ref_axis',(-1.,0.,0.));
#15504=DIRECTION('center_axis',(0.,0.,-1.));
#15505=DIRECTION('ref_axis',(1.,0.,0.));
#15506=DIRECTION('center_axis',(0.968133425390014,0.250434962899747,0.));
#15507=DIRECTION('ref_axis',(0.250434962899747,-0.968133425390014,0.));
#15508=DIRECTION('',(0.,0.,1.));
#15509=DIRECTION('',(0.250434962899747,-0.968133425390014,0.));
#15510=DIRECTION('',(0.,0.,-1.));
#15511=DIRECTION('',(0.250434962899747,-0.968133425390014,0.));
#15512=DIRECTION('center_axis',(0.,0.,1.));
#15513=DIRECTION('ref_axis',(1.,0.,0.));
#15514=DIRECTION('center_axis',(0.,0.,1.));
#15515=DIRECTION('ref_axis',(1.,0.,0.));
#15516=DIRECTION('',(-0.909937728342725,0.414744898146415,0.));
#15517=DIRECTION('center_axis',(-0.414744898146415,-0.909937728342725,0.));
#15518=DIRECTION('ref_axis',(-0.909937728342725,0.414744898146415,0.));
#15519=DIRECTION('',(0.,0.,-1.));
#15520=DIRECTION('',(-0.909937728342725,0.414744898146415,0.));
#15521=DIRECTION('center_axis',(0.,0.,-1.));
#15522=DIRECTION('ref_axis',(-1.,0.,0.));
#15523=DIRECTION('center_axis',(0.,0.,-1.));
#15524=DIRECTION('ref_axis',(1.,0.,0.));
#15525=DIRECTION('center_axis',(0.995401637679911,-0.0957892462865797,0.));
#15526=DIRECTION('ref_axis',(-0.0957892462865797,-0.995401637679911,0.));
#15527=DIRECTION('',(0.,0.,1.));
#15528=DIRECTION('',(-0.0957892462865797,-0.995401637679911,0.));
#15529=DIRECTION('',(0.,0.,-1.));
#15530=DIRECTION('',(-0.0957892462865797,-0.995401637679911,0.));
#15531=DIRECTION('center_axis',(0.,0.,1.));
#15532=DIRECTION('ref_axis',(1.,0.,0.));
#15533=DIRECTION('center_axis',(0.,0.,1.));
#15534=DIRECTION('ref_axis',(1.,0.,0.));
#15535=DIRECTION('',(-0.713210659190727,0.700949752562,0.));
#15536=DIRECTION('center_axis',(-0.700949752562,-0.713210659190727,0.));
#15537=DIRECTION('ref_axis',(-0.713210659190727,0.700949752562,0.));
#15538=DIRECTION('',(0.,0.,-1.));
#15539=DIRECTION('',(-0.713210659190727,0.700949752562,0.));
#15540=DIRECTION('center_axis',(0.,0.,-1.));
#15541=DIRECTION('ref_axis',(-1.,0.,0.));
#15542=DIRECTION('center_axis',(0.,0.,-1.));
#15543=DIRECTION('ref_axis',(1.,0.,0.));
#15544=DIRECTION('center_axis',(0.902609721902027,-0.430459858672031,0.));
#15545=DIRECTION('ref_axis',(-0.430459858672031,-0.902609721902027,0.));
#15546=DIRECTION('',(0.,0.,1.));
#15547=DIRECTION('',(-0.430459858672031,-0.902609721902027,0.));
#15548=DIRECTION('',(0.,0.,-1.));
#15549=DIRECTION('',(-0.430459858672031,-0.902609721902027,0.));
#15550=DIRECTION('center_axis',(0.,0.,1.));
#15551=DIRECTION('ref_axis',(1.,0.,0.));
#15552=DIRECTION('center_axis',(0.,0.,1.));
#15553=DIRECTION('ref_axis',(1.,0.,0.));
#15554=DIRECTION('',(-0.430459858672031,0.902609721902027,0.));
#15555=DIRECTION('center_axis',(-0.902609721902027,-0.430459858672031,0.));
#15556=DIRECTION('ref_axis',(-0.430459858672031,0.902609721902027,0.));
#15557=DIRECTION('',(0.,0.,-1.));
#15558=DIRECTION('',(-0.430459858672031,0.902609721902027,0.));
#15559=DIRECTION('center_axis',(0.,0.,-1.));
#15560=DIRECTION('ref_axis',(-1.,0.,0.));
#15561=DIRECTION('center_axis',(0.,0.,-1.));
#15562=DIRECTION('ref_axis',(1.,0.,0.));
#15563=DIRECTION('center_axis',(0.700949752562001,-0.713210659190726,0.));
#15564=DIRECTION('ref_axis',(-0.713210659190726,-0.700949752562001,0.));
#15565=DIRECTION('',(0.,0.,1.));
#15566=DIRECTION('',(-0.713210659190726,-0.700949752562001,0.));
#15567=DIRECTION('',(0.,0.,-1.));
#15568=DIRECTION('',(-0.713210659190726,-0.700949752562001,0.));
#15569=DIRECTION('center_axis',(0.,0.,1.));
#15570=DIRECTION('ref_axis',(1.,0.,0.));
#15571=DIRECTION('center_axis',(0.,0.,1.));
#15572=DIRECTION('ref_axis',(1.,0.,0.));
#15573=DIRECTION('',(-0.0957892462865797,0.995401637679911,0.));
#15574=DIRECTION('center_axis',(-0.995401637679911,-0.0957892462865797,
0.));
#15575=DIRECTION('ref_axis',(-0.0957892462865797,0.995401637679911,0.));
#15576=DIRECTION('',(0.,0.,-1.));
#15577=DIRECTION('',(-0.0957892462865797,0.995401637679911,0.));
#15578=DIRECTION('center_axis',(0.,0.,-1.));
#15579=DIRECTION('ref_axis',(-1.,0.,0.));
#15580=DIRECTION('center_axis',(0.,0.,-1.));
#15581=DIRECTION('ref_axis',(1.,0.,0.));
#15582=DIRECTION('center_axis',(0.414744898146414,-0.909937728342726,0.));
#15583=DIRECTION('ref_axis',(-0.909937728342726,-0.414744898146414,0.));
#15584=DIRECTION('',(0.,0.,1.));
#15585=DIRECTION('',(-0.909937728342726,-0.414744898146414,0.));
#15586=DIRECTION('',(0.,0.,-1.));
#15587=DIRECTION('',(-0.909937728342726,-0.414744898146414,0.));
#15588=DIRECTION('center_axis',(0.,0.,1.));
#15589=DIRECTION('ref_axis',(1.,0.,0.));
#15590=DIRECTION('center_axis',(0.,0.,1.));
#15591=DIRECTION('ref_axis',(1.,0.,0.));
#15592=DIRECTION('',(0.250434962899747,0.968133425390014,0.));
#15593=DIRECTION('center_axis',(-0.968133425390014,0.250434962899747,0.));
#15594=DIRECTION('ref_axis',(0.250434962899747,0.968133425390014,0.));
#15595=DIRECTION('',(0.,0.,-1.));
#15596=DIRECTION('',(0.250434962899747,0.968133425390014,0.));
#15597=DIRECTION('center_axis',(0.,0.,-1.));
#15598=DIRECTION('ref_axis',(-1.,0.,0.));
#15599=DIRECTION('center_axis',(0.,0.,-1.));
#15600=DIRECTION('ref_axis',(1.,0.,0.));
#15601=DIRECTION('center_axis',(0.078515688031576,-0.996912878205979,0.));
#15602=DIRECTION('ref_axis',(-0.996912878205979,-0.078515688031576,0.));
#15603=DIRECTION('',(0.,0.,1.));
#15604=DIRECTION('',(-0.996912878205979,-0.078515688031576,0.));
#15605=DIRECTION('',(0.,0.,-1.));
#15606=DIRECTION('',(-0.996912878205979,-0.078515688031576,0.));
#15607=DIRECTION('center_axis',(0.,0.,1.));
#15608=DIRECTION('ref_axis',(1.,0.,0.));
#15609=DIRECTION('center_axis',(0.,0.,1.));
#15610=DIRECTION('ref_axis',(1.,0.,0.));
#15611=DIRECTION('',(0.566453019533946,0.824094033870453,0.));
#15612=DIRECTION('center_axis',(-0.824094033870453,0.566453019533946,0.));
#15613=DIRECTION('ref_axis',(0.566453019533946,0.824094033870453,0.));
#15614=DIRECTION('',(0.,0.,-1.));
#15615=DIRECTION('',(0.566453019533946,0.824094033870453,0.));
#15616=DIRECTION('center_axis',(0.,0.,-1.));
#15617=DIRECTION('ref_axis',(-1.,0.,0.));
#15618=DIRECTION('center_axis',(0.,0.,-1.));
#15619=DIRECTION('ref_axis',(1.,0.,0.));
#15620=DIRECTION('center_axis',(-0.267183672828014,-0.963645622090472,0.));
#15621=DIRECTION('ref_axis',(-0.963645622090472,0.267183672828014,0.));
#15622=DIRECTION('',(0.,0.,1.));
#15623=DIRECTION('',(-0.963645622090472,0.267183672828014,0.));
#15624=DIRECTION('',(0.,0.,-1.));
#15625=DIRECTION('',(-0.963645622090472,0.267183672828014,0.));
#15626=DIRECTION('center_axis',(0.,0.,1.));
#15627=DIRECTION('ref_axis',(1.,0.,0.));
#15628=DIRECTION('center_axis',(0.,0.,1.));
#15629=DIRECTION('ref_axis',(1.,0.,0.));
#15630=DIRECTION('',(0.814148482056147,0.580656739533497,0.));
#15631=DIRECTION('center_axis',(-0.580656739533497,0.814148482056147,0.));
#15632=DIRECTION('ref_axis',(0.814148482056147,0.580656739533497,0.));
#15633=DIRECTION('',(0.,0.,-1.));
#15634=DIRECTION('',(0.814148482056147,0.580656739533497,0.));
#15635=DIRECTION('center_axis',(0.,0.,-1.));
#15636=DIRECTION('ref_axis',(-1.,0.,0.));
#15637=DIRECTION('center_axis',(0.,0.,-1.));
#15638=DIRECTION('ref_axis',(1.,0.,0.));
#15639=DIRECTION('center_axis',(-0.0957892462865788,-0.995401637679911,
0.));
#15640=DIRECTION('ref_axis',(-0.995401637679911,0.0957892462865788,0.));
#15641=DIRECTION('',(0.,0.,1.));
#15642=DIRECTION('',(-0.995401637679911,0.0957892462865788,0.));
#15643=DIRECTION('',(0.,0.,-1.));
#15644=DIRECTION('',(-0.995401637679911,0.0957892462865788,0.));
#15645=DIRECTION('center_axis',(0.,0.,1.));
#15646=DIRECTION('ref_axis',(1.,0.,0.));
#15647=DIRECTION('center_axis',(0.,0.,1.));
#15648=DIRECTION('ref_axis',(1.,0.,0.));
#15649=DIRECTION('',(0.700949752562,0.713210659190726,0.));
#15650=DIRECTION('center_axis',(-0.713210659190726,0.700949752562,0.));
#15651=DIRECTION('ref_axis',(0.700949752562,0.713210659190726,0.));
#15652=DIRECTION('',(0.,0.,-1.));
#15653=DIRECTION('',(0.700949752562,0.713210659190726,0.));
#15654=DIRECTION('center_axis',(0.,0.,-1.));
#15655=DIRECTION('ref_axis',(-1.,0.,0.));
#15656=DIRECTION('center_axis',(0.,0.,-1.));
#15657=DIRECTION('ref_axis',(1.,0.,0.));
#15658=DIRECTION('center_axis',(0.250434962899746,-0.968133425390014,0.));
#15659=DIRECTION('ref_axis',(-0.968133425390014,-0.250434962899746,0.));
#15660=DIRECTION('',(0.,0.,1.));
#15661=DIRECTION('',(-0.968133425390014,-0.250434962899746,0.));
#15662=DIRECTION('',(0.,0.,-1.));
#15663=DIRECTION('',(-0.968133425390014,-0.250434962899746,0.));
#15664=DIRECTION('center_axis',(0.,0.,1.));
#15665=DIRECTION('ref_axis',(1.,0.,0.));
#15666=DIRECTION('center_axis',(0.,0.,1.));
#15667=DIRECTION('ref_axis',(1.,0.,0.));
#15668=DIRECTION('',(0.414744898146414,0.909937728342726,0.));
#15669=DIRECTION('center_axis',(-0.909937728342726,0.414744898146414,0.));
#15670=DIRECTION('ref_axis',(0.414744898146414,0.909937728342726,0.));
#15671=DIRECTION('',(0.,0.,-1.));
#15672=DIRECTION('',(0.414744898146414,0.909937728342726,0.));
#15673=DIRECTION('center_axis',(0.,0.,-1.));
#15674=DIRECTION('ref_axis',(-1.,0.,0.));
#15675=DIRECTION('center_axis',(0.,0.,-1.));
#15676=DIRECTION('ref_axis',(1.,0.,0.));
#15677=DIRECTION('center_axis',(0.566453019533948,-0.824094033870452,0.));
#15678=DIRECTION('ref_axis',(-0.824094033870452,-0.566453019533948,0.));
#15679=DIRECTION('',(0.,0.,1.));
#15680=DIRECTION('',(-0.824094033870452,-0.566453019533948,0.));
#15681=DIRECTION('',(0.,0.,-1.));
#15682=DIRECTION('',(-0.824094033870452,-0.566453019533948,0.));
#15683=DIRECTION('center_axis',(0.,0.,1.));
#15684=DIRECTION('ref_axis',(1.,0.,0.));
#15685=DIRECTION('center_axis',(0.,0.,1.));
#15686=DIRECTION('ref_axis',(1.,0.,0.));
#15687=DIRECTION('',(0.0785156880315752,0.996912878205979,0.));
#15688=DIRECTION('center_axis',(-0.996912878205979,0.0785156880315752,0.));
#15689=DIRECTION('ref_axis',(0.0785156880315752,0.996912878205979,0.));
#15690=DIRECTION('',(0.,0.,-1.));
#15691=DIRECTION('',(0.0785156880315752,0.996912878205979,0.));
#15692=DIRECTION('center_axis',(0.,0.,-1.));
#15693=DIRECTION('ref_axis',(-1.,0.,0.));
#15694=DIRECTION('center_axis',(0.,0.,-1.));
#15695=DIRECTION('ref_axis',(1.,0.,0.));
#15696=DIRECTION('center_axis',(0.814148482056148,-0.580656739533496,0.));
#15697=DIRECTION('ref_axis',(-0.580656739533496,-0.814148482056148,0.));
#15698=DIRECTION('',(0.,0.,1.));
#15699=DIRECTION('',(-0.580656739533496,-0.814148482056148,0.));
#15700=DIRECTION('',(0.,0.,-1.));
#15701=DIRECTION('',(-0.580656739533496,-0.814148482056148,0.));
#15702=DIRECTION('center_axis',(0.,0.,1.));
#15703=DIRECTION('ref_axis',(1.,0.,0.));
#15704=DIRECTION('center_axis',(0.,0.,1.));
#15705=DIRECTION('ref_axis',(1.,0.,0.));
#15706=DIRECTION('',(-0.267183672828014,0.963645622090472,0.));
#15707=DIRECTION('center_axis',(-0.963645622090472,-0.267183672828014,0.));
#15708=DIRECTION('ref_axis',(-0.267183672828014,0.963645622090472,0.));
#15709=DIRECTION('',(0.,0.,-1.));
#15710=DIRECTION('',(-0.267183672828014,0.963645622090472,0.));
#15711=DIRECTION('center_axis',(0.,0.,-1.));
#15712=DIRECTION('ref_axis',(-1.,0.,0.));
#15713=DIRECTION('center_axis',(0.,0.,-1.));
#15714=DIRECTION('ref_axis',(1.,0.,0.));
#15715=DIRECTION('center_axis',(0.963645622090472,-0.267183672828014,0.));
#15716=DIRECTION('ref_axis',(-0.267183672828014,-0.963645622090472,0.));
#15717=DIRECTION('',(0.,0.,1.));
#15718=DIRECTION('',(-0.267183672828014,-0.963645622090472,0.));
#15719=DIRECTION('',(0.,0.,-1.));
#15720=DIRECTION('',(-0.267183672828014,-0.963645622090472,0.));
#15721=DIRECTION('center_axis',(0.,0.,1.));
#15722=DIRECTION('ref_axis',(1.,0.,0.));
#15723=DIRECTION('center_axis',(0.,0.,1.));
#15724=DIRECTION('ref_axis',(1.,0.,0.));
#15725=DIRECTION('',(-0.580656739533497,0.814148482056147,0.));
#15726=DIRECTION('center_axis',(-0.814148482056147,-0.580656739533497,0.));
#15727=DIRECTION('ref_axis',(-0.580656739533497,0.814148482056147,0.));
#15728=DIRECTION('',(0.,0.,-1.));
#15729=DIRECTION('',(-0.580656739533497,0.814148482056147,0.));
#15730=DIRECTION('center_axis',(0.,0.,-1.));
#15731=DIRECTION('ref_axis',(-1.,0.,0.));
#15732=DIRECTION('center_axis',(0.,0.,-1.));
#15733=DIRECTION('ref_axis',(1.,0.,0.));
#15734=DIRECTION('center_axis',(0.996912878205979,0.078515688031576,0.));
#15735=DIRECTION('ref_axis',(0.078515688031576,-0.996912878205979,0.));
#15736=DIRECTION('',(0.,0.,1.));
#15737=DIRECTION('',(0.078515688031576,-0.996912878205979,0.));
#15738=DIRECTION('',(0.,0.,-1.));
#15739=DIRECTION('',(0.078515688031576,-0.996912878205979,0.));
#15740=DIRECTION('center_axis',(0.,0.,1.));
#15741=DIRECTION('ref_axis',(1.,0.,0.));
#15742=DIRECTION('center_axis',(0.,0.,1.));
#15743=DIRECTION('ref_axis',(1.,0.,0.));
#15744=DIRECTION('',(-0.824094033870453,0.566453019533946,0.));
#15745=DIRECTION('center_axis',(-0.566453019533946,-0.824094033870453,0.));
#15746=DIRECTION('ref_axis',(-0.824094033870453,0.566453019533946,0.));
#15747=DIRECTION('',(0.,0.,-1.));
#15748=DIRECTION('',(-0.824094033870453,0.566453019533946,0.));
#15749=DIRECTION('center_axis',(0.,0.,-1.));
#15750=DIRECTION('ref_axis',(-1.,0.,0.));
#15751=DIRECTION('center_axis',(0.,0.,-1.));
#15752=DIRECTION('ref_axis',(1.,0.,0.));
#15753=DIRECTION('center_axis',(0.909937728342726,0.414744898146415,0.));
#15754=DIRECTION('ref_axis',(0.414744898146415,-0.909937728342726,0.));
#15755=DIRECTION('',(0.,0.,1.));
#15756=DIRECTION('',(0.414744898146415,-0.909937728342726,0.));
#15757=DIRECTION('',(0.,0.,-1.));
#15758=DIRECTION('',(0.414744898146415,-0.909937728342726,0.));
#15759=DIRECTION('center_axis',(0.,0.,1.));
#15760=DIRECTION('ref_axis',(1.,0.,0.));
#15761=DIRECTION('center_axis',(0.,0.,1.));
#15762=DIRECTION('ref_axis',(1.,0.,0.));
#15763=DIRECTION('',(-0.968133425390015,0.250434962899744,0.));
#15764=DIRECTION('center_axis',(-0.250434962899744,-0.968133425390015,0.));
#15765=DIRECTION('ref_axis',(-0.968133425390015,0.250434962899744,0.));
#15766=DIRECTION('',(0.,0.,-1.));
#15767=DIRECTION('',(-0.968133425390015,0.250434962899744,0.));
#15768=DIRECTION('center_axis',(0.,0.,-1.));
#15769=DIRECTION('ref_axis',(-1.,0.,0.));
#15770=DIRECTION('center_axis',(0.,0.,-1.));
#15771=DIRECTION('ref_axis',(1.,0.,0.));
#15772=DIRECTION('center_axis',(0.713210659190726,0.700949752562001,0.));
#15773=DIRECTION('ref_axis',(0.700949752562001,-0.713210659190726,0.));
#15774=DIRECTION('',(0.,0.,1.));
#15775=DIRECTION('',(0.700949752562001,-0.713210659190726,0.));
#15776=DIRECTION('',(0.,0.,-1.));
#15777=DIRECTION('',(0.700949752562001,-0.713210659190726,0.));
#15778=DIRECTION('center_axis',(0.,0.,1.));
#15779=DIRECTION('ref_axis',(1.,0.,0.));
#15780=DIRECTION('center_axis',(0.,0.,1.));
#15781=DIRECTION('ref_axis',(1.,0.,0.));
#15782=DIRECTION('',(-0.995401637679911,-0.0957892462865814,0.));
#15783=DIRECTION('center_axis',(0.0957892462865814,-0.995401637679911,0.));
#15784=DIRECTION('ref_axis',(-0.995401637679911,-0.0957892462865814,0.));
#15785=DIRECTION('',(0.,0.,-1.));
#15786=DIRECTION('',(-0.995401637679911,-0.0957892462865814,0.));
#15787=DIRECTION('center_axis',(0.,0.,-1.));
#15788=DIRECTION('ref_axis',(-1.,0.,0.));
#15789=DIRECTION('center_axis',(0.,0.,-1.));
#15790=DIRECTION('ref_axis',(1.,0.,0.));
#15791=DIRECTION('center_axis',(0.,0.,1.));
#15792=DIRECTION('ref_axis',(1.,0.,0.));
#15793=DIRECTION('center_axis',(0.,0.,1.));
#15794=DIRECTION('ref_axis',(1.,0.,0.));
#15795=DIRECTION('',(-0.902609721902027,0.430459858672031,0.));
#15796=DIRECTION('',(0.902609721902027,0.430459858672031,0.));
#15797=DIRECTION('center_axis',(-0.430459858672031,-0.902609721902027,0.));
#15798=DIRECTION('ref_axis',(-0.902609721902027,0.430459858672031,0.));
#15799=DIRECTION('',(0.,0.,1.));
#15800=DIRECTION('',(-0.902609721902027,0.430459858672031,0.));
#15801=DIRECTION('',(0.,0.,-1.));
#15802=DIRECTION('center_axis',(-0.430459858672031,0.902609721902027,0.));
#15803=DIRECTION('ref_axis',(0.902609721902027,0.430459858672031,0.));
#15804=DIRECTION('',(0.,0.,-1.));
#15805=DIRECTION('',(0.902609721902027,0.430459858672031,0.));
#15806=DIRECTION('center_axis',(0.,0.,-1.));
#15807=DIRECTION('ref_axis',(-1.,0.,0.));
#15808=DIRECTION('center_axis',(0.,0.,-1.));
#15809=DIRECTION('ref_axis',(1.,0.,0.));
#15810=DIRECTION('center_axis',(0.267183672828015,0.963645622090472,0.));
#15811=DIRECTION('ref_axis',(0.963645622090472,-0.267183672828015,0.));
#15812=DIRECTION('',(0.,0.,1.));
#15813=DIRECTION('',(0.963645622090472,-0.267183672828015,0.));
#15814=DIRECTION('',(0.,0.,-1.));
#15815=DIRECTION('',(0.963645622090472,-0.267183672828015,0.));
#15816=DIRECTION('center_axis',(0.,0.,1.));
#15817=DIRECTION('ref_axis',(1.,0.,0.));
#15818=DIRECTION('center_axis',(0.,0.,1.));
#15819=DIRECTION('ref_axis',(1.,0.,0.));
#15820=DIRECTION('',(-0.814148482056148,-0.580656739533496,0.));
#15821=DIRECTION('center_axis',(0.580656739533496,-0.814148482056148,0.));
#15822=DIRECTION('ref_axis',(-0.814148482056148,-0.580656739533496,0.));
#15823=DIRECTION('',(0.,0.,-1.));
#15824=DIRECTION('',(-0.814148482056148,-0.580656739533496,0.));
#15825=DIRECTION('center_axis',(0.,0.,-1.));
#15826=DIRECTION('ref_axis',(-1.,0.,0.));
#15827=DIRECTION('center_axis',(0.,0.,-1.));
#15828=DIRECTION('ref_axis',(1.,0.,0.));
#15829=DIRECTION('center_axis',(-0.0785156880315738,0.996912878205979,0.));
#15830=DIRECTION('ref_axis',(0.996912878205979,0.0785156880315738,0.));
#15831=DIRECTION('',(0.,0.,1.));
#15832=DIRECTION('',(0.996912878205979,0.0785156880315738,0.));
#15833=DIRECTION('',(0.,0.,-1.));
#15834=DIRECTION('',(0.996912878205979,0.0785156880315738,0.));
#15835=DIRECTION('center_axis',(0.,0.,1.));
#15836=DIRECTION('ref_axis',(1.,0.,0.));
#15837=DIRECTION('center_axis',(0.,0.,1.));
#15838=DIRECTION('ref_axis',(1.,0.,0.));
#15839=DIRECTION('',(-0.566453019533948,-0.824094033870452,0.));
#15840=DIRECTION('center_axis',(0.824094033870452,-0.566453019533948,0.));
#15841=DIRECTION('ref_axis',(-0.566453019533948,-0.824094033870452,0.));
#15842=DIRECTION('',(0.,0.,-1.));
#15843=DIRECTION('',(-0.566453019533948,-0.824094033870452,0.));
#15844=DIRECTION('center_axis',(0.,0.,-1.));
#15845=DIRECTION('ref_axis',(-1.,0.,0.));
#15846=DIRECTION('center_axis',(0.,0.,-1.));
#15847=DIRECTION('ref_axis',(1.,0.,0.));
#15848=DIRECTION('center_axis',(-0.414744898146415,0.909937728342726,0.));
#15849=DIRECTION('ref_axis',(0.909937728342726,0.414744898146415,0.));
#15850=DIRECTION('',(0.,0.,1.));
#15851=DIRECTION('',(0.909937728342726,0.414744898146415,0.));
#15852=DIRECTION('',(0.,0.,-1.));
#15853=DIRECTION('',(0.909937728342726,0.414744898146415,0.));
#15854=DIRECTION('center_axis',(0.,0.,1.));
#15855=DIRECTION('ref_axis',(1.,0.,0.));
#15856=DIRECTION('center_axis',(0.,0.,1.));
#15857=DIRECTION('ref_axis',(1.,0.,0.));
#15858=DIRECTION('',(-0.250434962899745,-0.968133425390015,0.));
#15859=DIRECTION('center_axis',(0.968133425390015,-0.250434962899745,0.));
#15860=DIRECTION('ref_axis',(-0.250434962899745,-0.968133425390015,0.));
#15861=DIRECTION('',(0.,0.,-1.));
#15862=DIRECTION('',(-0.250434962899745,-0.968133425390015,0.));
#15863=DIRECTION('center_axis',(0.,0.,-1.));
#15864=DIRECTION('ref_axis',(-1.,0.,0.));
#15865=DIRECTION('center_axis',(0.,0.,-1.));
#15866=DIRECTION('ref_axis',(1.,0.,0.));
#15867=DIRECTION('center_axis',(-0.700949752561999,0.713210659190727,0.));
#15868=DIRECTION('ref_axis',(0.713210659190727,0.700949752561999,0.));
#15869=DIRECTION('',(0.,0.,1.));
#15870=DIRECTION('',(0.713210659190727,0.700949752561999,0.));
#15871=DIRECTION('',(0.,0.,-1.));
#15872=DIRECTION('',(0.713210659190727,0.700949752561999,0.));
#15873=DIRECTION('center_axis',(0.,0.,1.));
#15874=DIRECTION('ref_axis',(1.,0.,0.));
#15875=DIRECTION('center_axis',(0.,0.,1.));
#15876=DIRECTION('ref_axis',(1.,0.,0.));
#15877=DIRECTION('',(0.0957892462865748,-0.995401637679912,0.));
#15878=DIRECTION('center_axis',(0.995401637679912,0.0957892462865748,0.));
#15879=DIRECTION('ref_axis',(0.0957892462865748,-0.995401637679912,0.));
#15880=DIRECTION('',(0.,0.,-1.));
#15881=DIRECTION('',(0.0957892462865748,-0.995401637679912,0.));
#15882=DIRECTION('center_axis',(0.,0.,-1.));
#15883=DIRECTION('ref_axis',(-1.,0.,0.));
#15884=DIRECTION('center_axis',(0.,0.,-1.));
#15885=DIRECTION('ref_axis',(1.,0.,0.));
#15886=DIRECTION('center_axis',(-0.902609721902026,0.430459858672033,0.));
#15887=DIRECTION('ref_axis',(0.430459858672033,0.902609721902026,0.));
#15888=DIRECTION('',(0.,0.,1.));
#15889=DIRECTION('',(0.430459858672033,0.902609721902026,0.));
#15890=DIRECTION('',(0.,0.,-1.));
#15891=DIRECTION('',(0.430459858672033,0.902609721902026,0.));
#15892=DIRECTION('center_axis',(0.,0.,1.));
#15893=DIRECTION('ref_axis',(1.,0.,0.));
#15894=DIRECTION('center_axis',(0.,0.,1.));
#15895=DIRECTION('ref_axis',(1.,0.,0.));
#15896=DIRECTION('',(0.430459858672033,-0.902609721902027,0.));
#15897=DIRECTION('center_axis',(0.902609721902027,0.430459858672033,0.));
#15898=DIRECTION('ref_axis',(0.430459858672033,-0.902609721902027,0.));
#15899=DIRECTION('',(0.,0.,-1.));
#15900=DIRECTION('',(0.430459858672033,-0.902609721902027,0.));
#15901=DIRECTION('center_axis',(0.,0.,-1.));
#15902=DIRECTION('ref_axis',(-1.,0.,0.));
#15903=DIRECTION('center_axis',(0.,0.,-1.));
#15904=DIRECTION('ref_axis',(1.,0.,0.));
#15905=DIRECTION('center_axis',(-0.995401637679911,0.0957892462865809,0.));
#15906=DIRECTION('ref_axis',(0.0957892462865809,0.995401637679911,0.));
#15907=DIRECTION('',(0.,0.,1.));
#15908=DIRECTION('',(0.0957892462865809,0.995401637679911,0.));
#15909=DIRECTION('',(0.,0.,-1.));
#15910=DIRECTION('',(0.0957892462865809,0.995401637679911,0.));
#15911=DIRECTION('center_axis',(0.,0.,1.));
#15912=DIRECTION('ref_axis',(1.,0.,0.));
#15913=DIRECTION('center_axis',(0.,0.,1.));
#15914=DIRECTION('ref_axis',(1.,0.,0.));
#15915=DIRECTION('',(0.713210659190723,-0.700949752562004,0.));
#15916=DIRECTION('center_axis',(0.700949752562004,0.713210659190723,0.));
#15917=DIRECTION('ref_axis',(0.713210659190723,-0.700949752562004,0.));
#15918=DIRECTION('',(0.,0.,-1.));
#15919=DIRECTION('',(0.713210659190723,-0.700949752562004,0.));
#15920=DIRECTION('center_axis',(0.,0.,-1.));
#15921=DIRECTION('ref_axis',(-1.,0.,0.));
#15922=DIRECTION('center_axis',(0.,0.,-1.));
#15923=DIRECTION('ref_axis',(1.,0.,0.));
#15924=DIRECTION('center_axis',(-0.968133425390015,-0.250434962899744,0.));
#15925=DIRECTION('ref_axis',(-0.250434962899744,0.968133425390015,0.));
#15926=DIRECTION('',(0.,0.,1.));
#15927=DIRECTION('',(-0.250434962899744,0.968133425390015,0.));
#15928=DIRECTION('',(0.,0.,-1.));
#15929=DIRECTION('',(-0.250434962899744,0.968133425390015,0.));
#15930=DIRECTION('center_axis',(0.,0.,1.));
#15931=DIRECTION('ref_axis',(1.,0.,0.));
#15932=DIRECTION('center_axis',(0.,0.,1.));
#15933=DIRECTION('ref_axis',(1.,0.,0.));
#15934=DIRECTION('',(0.909937728342727,-0.414744898146412,0.));
#15935=DIRECTION('center_axis',(0.414744898146412,0.909937728342727,0.));
#15936=DIRECTION('ref_axis',(0.909937728342727,-0.414744898146412,0.));
#15937=DIRECTION('',(0.,0.,-1.));
#15938=DIRECTION('',(0.909937728342727,-0.414744898146412,0.));
#15939=DIRECTION('center_axis',(0.,0.,-1.));
#15940=DIRECTION('ref_axis',(-1.,0.,0.));
#15941=DIRECTION('center_axis',(0.,0.,-1.));
#15942=DIRECTION('ref_axis',(1.,0.,0.));
#15943=DIRECTION('center_axis',(-0.82409403387045,-0.56645301953395,0.));
#15944=DIRECTION('ref_axis',(-0.56645301953395,0.82409403387045,0.));
#15945=DIRECTION('',(0.,0.,1.));
#15946=DIRECTION('',(-0.56645301953395,0.82409403387045,0.));
#15947=DIRECTION('',(0.,0.,-1.));
#15948=DIRECTION('',(-0.56645301953395,0.82409403387045,0.));
#15949=DIRECTION('center_axis',(0.,0.,1.));
#15950=DIRECTION('ref_axis',(1.,0.,0.));
#15951=DIRECTION('center_axis',(0.,0.,1.));
#15952=DIRECTION('ref_axis',(1.,0.,0.));
#15953=DIRECTION('',(0.996912878205979,-0.0785156880315738,0.));
#15954=DIRECTION('center_axis',(0.0785156880315738,0.996912878205979,0.));
#15955=DIRECTION('ref_axis',(0.996912878205979,-0.0785156880315738,0.));
#15956=DIRECTION('',(0.,0.,-1.));
#15957=DIRECTION('',(0.996912878205979,-0.0785156880315738,0.));
#15958=DIRECTION('center_axis',(0.,0.,-1.));
#15959=DIRECTION('ref_axis',(-1.,0.,0.));
#15960=DIRECTION('center_axis',(0.,0.,-1.));
#15961=DIRECTION('ref_axis',(1.,0.,0.));
#15962=DIRECTION('center_axis',(-0.580656739533499,-0.814148482056146,0.));
#15963=DIRECTION('ref_axis',(-0.814148482056146,0.580656739533499,0.));
#15964=DIRECTION('',(0.,0.,1.));
#15965=DIRECTION('',(-0.814148482056146,0.580656739533499,0.));
#15966=DIRECTION('',(0.,0.,-1.));
#15967=DIRECTION('',(-0.814148482056146,0.580656739533499,0.));
#15968=DIRECTION('center_axis',(0.,0.,1.));
#15969=DIRECTION('ref_axis',(1.,0.,0.));
#15970=DIRECTION('center_axis',(0.,0.,1.));
#15971=DIRECTION('ref_axis',(1.,0.,0.));
#15972=DIRECTION('',(0.963645622090472,0.267183672828016,0.));
#15973=DIRECTION('center_axis',(-0.267183672828016,0.963645622090472,0.));
#15974=DIRECTION('ref_axis',(0.963645622090472,0.267183672828016,0.));
#15975=DIRECTION('',(0.,0.,-1.));
#15976=DIRECTION('',(0.963645622090472,0.267183672828016,0.));
#15977=DIRECTION('center_axis',(0.,0.,-1.));
#15978=DIRECTION('ref_axis',(-1.,0.,0.));
#15979=DIRECTION('center_axis',(0.,0.,-1.));
#15980=DIRECTION('ref_axis',(1.,0.,0.));
#15981=DIRECTION('center_axis',(0.,0.,1.));
#15982=DIRECTION('ref_axis',(1.,0.,0.));
#15983=DIRECTION('center_axis',(0.,0.,1.));
#15984=DIRECTION('ref_axis',(-1.,1.22464679914735E-16,0.));
#15985=DIRECTION('center_axis',(1.22464679914735E-16,-1.,0.));
#15986=DIRECTION('ref_axis',(-1.,-1.22464679914735E-16,0.));
#15987=DIRECTION('center_axis',(0.,0.,-1.));
#15988=DIRECTION('ref_axis',(-1.,1.22464679914735E-16,0.));
#15989=DIRECTION('center_axis',(0.,0.,1.));
#15990=DIRECTION('ref_axis',(1.,0.,0.));
#15991=DIRECTION('',(0.,0.,-1.));
#15992=DIRECTION('center_axis',(0.,0.,1.));
#15993=DIRECTION('ref_axis',(1.,0.,0.));
#15994=DIRECTION('center_axis',(0.,0.,-1.));
#15995=DIRECTION('ref_axis',(-1.,0.,0.));
#15996=DIRECTION('center_axis',(0.,0.,1.));
#15997=DIRECTION('ref_axis',(1.,0.,0.));
#15998=DIRECTION('center_axis',(0.,0.,-1.));
#15999=DIRECTION('ref_axis',(-1.,0.,0.));
#16000=DIRECTION('center_axis',(0.,0.,1.));
#16001=DIRECTION('ref_axis',(1.,0.,0.));
#16002=DIRECTION('center_axis',(0.,0.,1.));
#16003=DIRECTION('ref_axis',(1.,0.,0.));
#16004=DIRECTION('',(0.707106781186547,8.65956056235493E-17,-0.707106781186548));
#16005=DIRECTION('center_axis',(0.,0.,1.));
#16006=DIRECTION('ref_axis',(1.,0.,0.));
#16007=DIRECTION('center_axis',(0.,0.,-1.));
#16008=DIRECTION('ref_axis',(1.,0.,0.));
#16009=DIRECTION('center_axis',(0.,0.,1.));
#16010=DIRECTION('ref_axis',(1.,0.,0.));
#16011=DIRECTION('center_axis',(0.,0.,1.));
#16012=DIRECTION('ref_axis',(1.,0.,0.));
#16013=DIRECTION('center_axis',(0.,0.,1.));
#16014=DIRECTION('ref_axis',(1.,0.,0.));
#16015=DIRECTION('',(0.707106781186548,8.65956056235494E-17,-0.707106781186547));
#16016=DIRECTION('center_axis',(0.,0.,1.));
#16017=DIRECTION('ref_axis',(1.,0.,0.));
#16018=DIRECTION('center_axis',(0.,0.,1.));
#16019=DIRECTION('ref_axis',(1.,0.,0.));
#16020=DIRECTION('center_axis',(0.,0.,1.));
#16021=DIRECTION('ref_axis',(1.,0.,0.));
#16022=DIRECTION('center_axis',(0.,0.,1.));
#16023=DIRECTION('ref_axis',(1.,0.,0.));
#16024=DIRECTION('center_axis',(0.,0.,1.));
#16025=DIRECTION('ref_axis',(1.,0.,0.));
#16026=DIRECTION('center_axis',(0.,0.,1.));
#16027=DIRECTION('ref_axis',(1.,0.,0.));
#16028=DIRECTION('center_axis',(0.,0.,1.));
#16029=DIRECTION('ref_axis',(1.,0.,0.));
#16030=DIRECTION('center_axis',(0.,0.,1.));
#16031=DIRECTION('ref_axis',(1.,0.,0.));
#16032=DIRECTION('center_axis',(0.,0.,1.));
#16033=DIRECTION('ref_axis',(1.,0.,0.));
#16034=DIRECTION('center_axis',(0.,0.,1.));
#16035=DIRECTION('ref_axis',(1.,0.,0.));
#16036=DIRECTION('center_axis',(0.,0.,1.));
#16037=DIRECTION('ref_axis',(1.,0.,0.));
#16038=DIRECTION('center_axis',(0.,0.,1.));
#16039=DIRECTION('ref_axis',(1.,0.,0.));
#16040=DIRECTION('center_axis',(0.,0.,1.));
#16041=DIRECTION('ref_axis',(1.,0.,0.));
#16042=DIRECTION('center_axis',(0.,0.,1.));
#16043=DIRECTION('ref_axis',(1.,0.,0.));
#16044=DIRECTION('center_axis',(0.,0.,1.));
#16045=DIRECTION('ref_axis',(1.,0.,0.));
#16046=DIRECTION('center_axis',(0.,0.,1.));
#16047=DIRECTION('ref_axis',(1.,0.,0.));
#16048=DIRECTION('center_axis',(0.,0.,1.));
#16049=DIRECTION('ref_axis',(1.,0.,0.));
#16050=DIRECTION('',(0.,0.,-1.));
#16051=DIRECTION('center_axis',(0.,0.,1.));
#16052=DIRECTION('ref_axis',(1.,0.,0.));
#16053=DIRECTION('center_axis',(0.,0.,1.));
#16054=DIRECTION('ref_axis',(1.,0.,0.));
#16055=DIRECTION('center_axis',(0.,0.,1.));
#16056=DIRECTION('ref_axis',(1.,0.,0.));
#16057=DIRECTION('center_axis',(0.,0.,1.));
#16058=DIRECTION('ref_axis',(1.,0.,0.));
#16059=DIRECTION('center_axis',(0.,0.,1.));
#16060=DIRECTION('ref_axis',(1.,0.,0.));
#16061=DIRECTION('center_axis',(0.,0.,1.));
#16062=DIRECTION('ref_axis',(1.,0.,0.));
#16063=DIRECTION('center_axis',(0.,0.,1.));
#16064=DIRECTION('ref_axis',(1.,0.,0.));
#16065=DIRECTION('center_axis',(0.,0.,1.));
#16066=DIRECTION('ref_axis',(1.,0.,0.));
#16067=DIRECTION('center_axis',(0.,0.,1.));
#16068=DIRECTION('ref_axis',(1.,0.,0.));
#16069=DIRECTION('center_axis',(0.,0.,1.));
#16070=DIRECTION('ref_axis',(1.,0.,0.));
#16071=DIRECTION('center_axis',(0.,0.,1.));
#16072=DIRECTION('ref_axis',(1.,0.,0.));
#16073=DIRECTION('center_axis',(0.,0.,1.));
#16074=DIRECTION('ref_axis',(1.,0.,0.));
#16075=DIRECTION('center_axis',(0.,0.,1.));
#16076=DIRECTION('ref_axis',(1.,0.,0.));
#16077=DIRECTION('center_axis',(0.,0.,1.));
#16078=DIRECTION('ref_axis',(1.,0.,0.));
#16079=DIRECTION('center_axis',(0.,0.,1.));
#16080=DIRECTION('ref_axis',(1.,0.,0.));
#16081=DIRECTION('center_axis',(0.,0.,1.));
#16082=DIRECTION('ref_axis',(1.,0.,0.));
#16083=DIRECTION('center_axis',(0.,0.,1.));
#16084=DIRECTION('ref_axis',(1.,0.,0.));
#16085=DIRECTION('center_axis',(0.,0.,1.));
#16086=DIRECTION('ref_axis',(1.,0.,0.));
#16087=DIRECTION('center_axis',(0.,0.,1.));
#16088=DIRECTION('ref_axis',(1.,0.,0.));
#16089=DIRECTION('center_axis',(0.,0.,1.));
#16090=DIRECTION('ref_axis',(1.,0.,0.));
#16091=DIRECTION('center_axis',(0.,0.,-1.));
#16092=DIRECTION('ref_axis',(1.,0.,0.));
#16093=DIRECTION('center_axis',(0.,0.,1.));
#16094=DIRECTION('ref_axis',(1.,0.,0.));
#16095=DIRECTION('',(-0.707106781186547,-8.65956056235493E-17,-0.707106781186547));
#16096=DIRECTION('center_axis',(0.,0.,1.));
#16097=DIRECTION('ref_axis',(1.,0.,0.));
#16098=DIRECTION('axis',(0.,0.,1.));
#16099=DIRECTION('refdir',(1.,0.,0.));
#16100=DIRECTION('center_axis',(0.,0.,-1.));
#16101=DIRECTION('ref_axis',(-1.,0.,0.));
#16102=DIRECTION('center_axis',(0.,0.,-1.));
#16103=DIRECTION('ref_axis',(-1.,0.,0.));
#16104=DIRECTION('',(0.707106781186548,8.65956056235494E-17,-0.707106781186547));
#16105=DIRECTION('center_axis',(0.,0.,1.));
#16106=DIRECTION('ref_axis',(-1.,0.,0.));
#16107=DIRECTION('center_axis',(0.,0.,1.));
#16108=DIRECTION('ref_axis',(-1.,0.,0.));
#16109=DIRECTION('center_axis',(0.,0.,1.));
#16110=DIRECTION('ref_axis',(1.,0.,0.));
#16111=DIRECTION('center_axis',(0.,0.,1.));
#16112=DIRECTION('ref_axis',(-1.,0.,0.));
#16113=DIRECTION('center_axis',(0.,0.,1.));
#16114=DIRECTION('ref_axis',(1.,0.,0.));
#16115=DIRECTION('',(0.,0.,-1.));
#16116=DIRECTION('center_axis',(0.,0.,1.));
#16117=DIRECTION('ref_axis',(1.,0.,0.));
#16118=DIRECTION('center_axis',(0.,0.,-1.));
#16119=DIRECTION('ref_axis',(-1.,0.,0.));
#16120=DIRECTION('center_axis',(0.,0.,-1.));
#16121=DIRECTION('ref_axis',(-1.,0.,0.));
#16122=DIRECTION('',(-0.707106781186548,8.65956056235494E-17,0.707106781186547));
#16123=DIRECTION('center_axis',(0.,0.,1.));
#16124=DIRECTION('ref_axis',(-1.,0.,0.));
#16125=DIRECTION('center_axis',(0.,0.,1.));
#16126=DIRECTION('ref_axis',(-1.,0.,0.));
#16127=DIRECTION('center_axis',(0.,0.,1.));
#16128=DIRECTION('ref_axis',(1.,0.,0.));
#16129=DIRECTION('center_axis',(0.,0.,-1.));
#16130=DIRECTION('ref_axis',(-1.,0.,0.));
#16131=DIRECTION('center_axis',(0.,0.,-1.));
#16132=DIRECTION('ref_axis',(-1.,0.,0.));
#16133=DIRECTION('',(0.,0.,-1.));
#16134=DIRECTION('center_axis',(0.,0.,-1.));
#16135=DIRECTION('ref_axis',(-1.,0.,0.));
#16136=DIRECTION('center_axis',(0.,0.,1.));
#16137=DIRECTION('ref_axis',(1.,0.,0.));
#16138=DIRECTION('center_axis',(0.,0.,1.));
#16139=DIRECTION('ref_axis',(-1.,0.,0.));
#16140=DIRECTION('',(0.707106781186548,-8.65956056235494E-17,0.707106781186547));
#16141=DIRECTION('center_axis',(0.,0.,1.));
#16142=DIRECTION('ref_axis',(1.,0.,0.));
#16143=DIRECTION('',(0.707106781186548,8.65956056235494E-17,-0.707106781186547));
#16144=DIRECTION('axis',(0.,0.,1.));
#16145=DIRECTION('refdir',(1.,0.,0.));
#16146=DIRECTION('center_axis',(0.804732485689015,-0.464612517239211,0.369514323540269));
#16147=DIRECTION('ref_axis',(0.417287908209953,0.,-0.908774340340748));
#16148=DIRECTION('',(-0.499999999999997,-0.86602540378444,-6.10464344883671E-15));
#16149=DIRECTION('center_axis',(-8.89195164525175E-13,-0.929225034476892,
0.369514323540265));
#16150=DIRECTION('ref_axis',(0.,-0.369514323540265,-0.929225034476892));
#16151=DIRECTION('',(-1.,0.,-1.52616086220918E-15));
#16152=DIRECTION('center_axis',(0.804732485689902,0.464612517237679,0.369514323540264));
#16153=DIRECTION('ref_axis',(0.417287908209569,0.,-0.908774340340925));
#16154=DIRECTION('',(0.499999999999999,-0.866025403784439,-6.10464344883671E-15));
#16155=DIRECTION('center_axis',(-0.804732485689905,-0.464612517237674,0.369514323540265));
#16156=DIRECTION('ref_axis',(0.417287908209569,0.,0.908774340340924));
#16157=DIRECTION('',(-0.499999999999999,0.866025403784439,-3.05232172441835E-15));
#16158=DIRECTION('center_axis',(8.86349292865986E-13,0.92922503447689,0.369514323540268));
#16159=DIRECTION('ref_axis',(0.,-0.369514323540268,0.92922503447689));
#16160=DIRECTION('',(1.,3.05232172441836E-15,-4.57848258662754E-15));
#16161=DIRECTION('center_axis',(-0.804732485689018,0.464612517239214,0.369514323540261));
#16162=DIRECTION('ref_axis',(0.417287908209945,0.,0.908774340340752));
#16163=DIRECTION('',(0.499999999999999,0.866025403784439,-6.10464344883671E-15));
#16164=DIRECTION('center_axis',(-0.866025403784439,0.499999999999999,0.));
#16165=DIRECTION('ref_axis',(0.,0.,1.));
#16166=DIRECTION('',(0.,0.,1.));
#16167=DIRECTION('',(0.,0.,-1.));
#16168=DIRECTION('center_axis',(-3.05232172441836E-15,1.,0.));
#16169=DIRECTION('ref_axis',(0.,0.,1.));
#16170=DIRECTION('',(0.,0.,1.));
#16171=DIRECTION('',(0.,0.,-1.));
#16172=DIRECTION('center_axis',(-0.866025403784439,-0.499999999999999,0.));
#16173=DIRECTION('ref_axis',(0.,0.,1.));
#16174=DIRECTION('',(0.,0.,1.));
#16175=DIRECTION('',(0.,0.,-1.));
#16176=DIRECTION('center_axis',(0.866025403784439,0.499999999999999,0.));
#16177=DIRECTION('ref_axis',(0.,0.,-1.));
#16178=DIRECTION('',(0.,0.,1.));
#16179=DIRECTION('',(0.,0.,-1.));
#16180=DIRECTION('center_axis',(0.,-1.,0.));
#16181=DIRECTION('ref_axis',(0.,0.,-1.));
#16182=DIRECTION('',(0.,0.,1.));
#16183=DIRECTION('',(0.,0.,-1.));
#16184=DIRECTION('center_axis',(0.86602540378444,-0.499999999999997,0.));
#16185=DIRECTION('ref_axis',(0.,0.,-1.));
#16186=DIRECTION('',(0.,0.,1.));
#16187=DIRECTION('',(0.,0.,-1.));
#16188=DIRECTION('center_axis',(0.5,0.866025403784439,0.));
#16189=DIRECTION('ref_axis',(-0.866025403784439,0.5,0.));
#16190=DIRECTION('center_axis',(1.,-3.84592537276713E-16,0.));
#16191=DIRECTION('ref_axis',(3.84592537276713E-16,1.,0.));
#16192=DIRECTION('center_axis',(0.5,-0.866025403784439,0.));
#16193=DIRECTION('ref_axis',(0.866025403784439,0.5,0.));
#16194=DIRECTION('center_axis',(0.,0.,1.));
#16195=DIRECTION('ref_axis',(1.,0.,0.));
#16196=DIRECTION('center_axis',(0.,0.,-1.));
#16197=DIRECTION('ref_axis',(1.,0.,0.));
#16198=DIRECTION('',(-0.866025403784439,-1.06057523872491E-16,0.5));
#16199=DIRECTION('center_axis',(0.,0.,-1.));
#16200=DIRECTION('ref_axis',(1.,0.,0.));
#16201=DIRECTION('center_axis',(0.,0.,1.));
#16202=DIRECTION('ref_axis',(-1.,-6.12323399573677E-17,0.));
#16203=DIRECTION('center_axis',(0.,0.,-1.));
#16204=DIRECTION('ref_axis',(1.,0.,0.));
#16205=DIRECTION('center_axis',(0.,0.,1.));
#16206=DIRECTION('ref_axis',(-1.,-6.12323399573677E-17,0.));
#16207=DIRECTION('center_axis',(0.,0.,-1.));
#16208=DIRECTION('ref_axis',(1.,0.,0.));
#16209=DIRECTION('center_axis',(0.,0.,1.));
#16210=DIRECTION('ref_axis',(-1.,-6.12323399573677E-17,0.));
#16211=DIRECTION('center_axis',(0.,0.,-1.));
#16212=DIRECTION('ref_axis',(1.,0.,0.));
#16213=DIRECTION('center_axis',(0.,0.,1.));
#16214=DIRECTION('ref_axis',(-1.,-6.12323399573677E-17,0.));
#16215=DIRECTION('center_axis',(0.,0.,-1.));
#16216=DIRECTION('ref_axis',(1.,0.,0.));
#16217=DIRECTION('center_axis',(0.,0.,1.));
#16218=DIRECTION('ref_axis',(-1.,-6.12323399573677E-17,0.));
#16219=DIRECTION('center_axis',(0.,0.,-1.));
#16220=DIRECTION('ref_axis',(1.,0.,0.));
#16221=DIRECTION('center_axis',(0.,0.,1.));
#16222=DIRECTION('ref_axis',(-1.,-6.12323399573677E-17,0.));
#16223=DIRECTION('center_axis',(0.,-2.87609195051533E-15,-1.));
#16224=DIRECTION('ref_axis',(-1.,-3.18828070427431E-17,0.));
#16225=DIRECTION('center_axis',(0.,0.,-1.));
#16226=DIRECTION('ref_axis',(-1.,0.,0.));
#16227=DIRECTION('',(0.965925826289069,-5.95299148384376E-16,-0.25881904510252));
#16228=DIRECTION('center_axis',(0.,0.,1.));
#16229=DIRECTION('ref_axis',(1.,0.,0.));
#16230=DIRECTION('center_axis',(0.,0.,1.));
#16231=DIRECTION('ref_axis',(1.,0.,0.));
#16232=DIRECTION('center_axis',(0.,1.36140975242952E-15,1.));
#16233=DIRECTION('ref_axis',(1.,2.90395481232862E-17,0.));
#16234=DIRECTION('center_axis',(0.,0.,-1.));
#16235=DIRECTION('ref_axis',(1.,6.12323399573676E-17,0.));
#16236=DIRECTION('',(-0.923879532511287,6.07302523999323E-16,0.382683432365089));
#16237=DIRECTION('center_axis',(0.,0.,1.));
#16238=DIRECTION('ref_axis',(1.,0.,0.));
#16239=DIRECTION('',(0.707106781186547,8.65956056235493E-17,-0.707106781186548));
#16240=DIRECTION('center_axis',(0.,0.,1.));
#16241=DIRECTION('ref_axis',(1.,6.12323399573676E-17,0.));
#16242=DIRECTION('center_axis',(0.,-5.46318868466739E-16,1.));
#16243=DIRECTION('ref_axis',(1.,3.13437485667187E-17,0.));
#16244=DIRECTION('',(0.382683432365089,5.63592758139109E-16,-0.923879532511287));
#16245=DIRECTION('center_axis',(0.,0.,-1.));
#16246=DIRECTION('ref_axis',(1.,0.,0.));
#16247=DIRECTION('center_axis',(0.,0.,1.));
#16248=DIRECTION('ref_axis',(1.,0.,0.));
#16249=DIRECTION('',(0.,0.,-1.));
#16250=DIRECTION('center_axis',(0.,0.,1.));
#16251=DIRECTION('ref_axis',(1.,0.,0.));
#16252=DIRECTION('center_axis',(0.,0.,-1.));
#16253=DIRECTION('ref_axis',(1.,0.,0.));
#16254=DIRECTION('',(-0.707106781186547,-8.65956056235493E-17,-0.707106781186548));
#16255=DIRECTION('center_axis',(0.,0.,-1.));
#16256=DIRECTION('ref_axis',(1.,0.,0.));
#16257=DIRECTION('center_axis',(0.,0.,1.));
#16258=DIRECTION('ref_axis',(1.,0.,0.));
#16259=DIRECTION('center_axis',(-0.5,-0.866025403784439,0.));
#16260=DIRECTION('ref_axis',(0.866025403784439,-0.5,0.));
#16261=DIRECTION('center_axis',(-1.,-1.92296268638356E-16,0.));
#16262=DIRECTION('ref_axis',(1.92296268638356E-16,-1.,0.));
#16263=DIRECTION('center_axis',(-0.5,0.866025403784439,0.));
#16264=DIRECTION('ref_axis',(-0.866025403784439,-0.5,0.));
#16265=DIRECTION('',(0.,0.,1.));
#16266=DIRECTION('',(1.,0.,0.));
#16267=DIRECTION('',(0.,0.,1.));
#16268=DIRECTION('',(0.987688340595138,-0.15643446504023,0.));
#16269=DIRECTION('',(0.,0.,1.));
#16270=DIRECTION('',(0.987688340595138,-0.156434465040231,0.));
#16271=DIRECTION('',(1.,6.47112461314111E-32,-2.22044604925031E-16));
#16272=DIRECTION('',(-2.22044604925031E-16,2.91433543964104E-16,-1.));
#16273=DIRECTION('',(0.,0.,1.));
#16274=DIRECTION('',(1.,0.,0.));
#16275=DIRECTION('',(0.,0.,1.));
#16276=DIRECTION('',(0.987688340595138,-0.156434465040231,0.));
#16277=DIRECTION('',(0.,0.,1.));
#16278=DIRECTION('',(0.987688340595138,-0.15643446504023,0.));
#16279=DIRECTION('',(0.,0.,1.));
#16280=DIRECTION('',(0.987688340595138,-0.156434465040231,0.));
#16281=DIRECTION('',(0.,-1.,-2.22044604925031E-16));
#16282=DIRECTION('',(1.,0.,0.));
#16283=DIRECTION('',(0.,1.,-2.22044604925031E-16));
#16284=DIRECTION('',(1.,0.,0.));
#16285=DIRECTION('',(0.,1.,-2.22044604925031E-16));
#16286=DIRECTION('',(1.,0.,0.));
#16287=DIRECTION('',(1.,-2.1570415377137E-32,-2.22044604925031E-16));
#16288=DIRECTION('',(-2.22044604925031E-16,-9.71445146547012E-17,-1.));
#16289=DIRECTION('',(-1.,2.1570415377137E-32,-2.22044604925031E-16));
#16290=DIRECTION('',(-2.22044604925031E-16,-9.71445146547012E-17,1.));
#16291=DIRECTION('',(-1.,2.1570415377137E-32,-2.22044604925031E-16));
#16292=DIRECTION('',(-2.22044604925031E-16,-9.71445146547012E-17,1.));
#16293=DIRECTION('',(0.,0.,1.));
#16294=DIRECTION('',(1.,0.,0.));
#16295=DIRECTION('',(1.,0.,-2.22044604925031E-16));
#16296=DIRECTION('',(-2.22044604925031E-16,0.,-1.));
#16297=DIRECTION('',(1.,0.,-2.22044604925031E-16));
#16298=DIRECTION('',(-2.22044604925031E-16,0.,-1.));
#16299=DIRECTION('',(-1.,0.,-2.22044604925031E-16));
#16300=DIRECTION('',(-2.22044604925031E-16,0.,1.));
#16301=DIRECTION('',(-1.,0.,-2.22044604925031E-16));
#16302=DIRECTION('',(-2.22044604925031E-16,0.,1.));
#16303=DIRECTION('',(1.,-2.1570415377137E-32,-2.22044604925031E-16));
#16304=DIRECTION('',(-2.22044604925031E-16,-9.71445146547012E-17,-1.));
#16305=DIRECTION('',(-1.,2.1570415377137E-32,-2.22044604925031E-16));
#16306=DIRECTION('',(-2.22044604925031E-16,-9.71445146547012E-17,1.));
#16307=DIRECTION('',(1.,-2.1570415377137E-32,-2.22044604925031E-16));
#16308=DIRECTION('',(-2.22044604925031E-16,-9.71445146547012E-17,-1.));
#16309=DIRECTION('',(-1.,2.1570415377137E-32,-2.22044604925031E-16));
#16310=DIRECTION('',(-2.22044604925031E-16,-9.71445146547012E-17,1.));
#16311=DIRECTION('',(0.,0.,1.));
#16312=DIRECTION('',(0.15643446504023,0.987688340595138,0.));
#16313=DIRECTION('',(1.,-2.1570415377137E-32,-2.22044604925031E-16));
#16314=DIRECTION('',(-2.22044604925031E-16,-9.71445146547012E-17,-1.));
#16315=DIRECTION('',(1.,8.62816615085482E-32,-2.22044604925031E-16));
#16316=DIRECTION('',(4.46783074719278E-32,1.,4.44089209850062E-16));
#16317=DIRECTION('',(-1.,2.1570415377137E-32,-2.22044604925031E-16));
#16318=DIRECTION('',(-2.22044604925031E-16,-9.71445146547012E-17,1.));
#16319=DIRECTION('',(-1.,-8.62816615085482E-32,-2.22044604925031E-16));
#16320=DIRECTION('',(4.46783074719278E-32,1.,-4.44089209850062E-16));
#16321=DIRECTION('',(0.,-1.,-2.22044604925031E-16));
#16322=DIRECTION('',(1.,0.,0.));
#16323=DIRECTION('',(0.,-1.,-2.22044604925031E-16));
#16324=DIRECTION('',(1.,0.,0.));
#16325=DIRECTION('',(0.,-1.,-2.22044604925031E-16));
#16326=DIRECTION('',(1.,0.,0.));
#16327=DIRECTION('',(0.,1.,-2.22044604925031E-16));
#16328=DIRECTION('',(1.,0.,0.));
#16329=DIRECTION('',(0.,1.,-2.22044604925031E-16));
#16330=DIRECTION('',(1.,0.,0.));
#16331=DIRECTION('',(0.,1.,-2.22044604925031E-16));
#16332=DIRECTION('',(1.,0.,0.));
#16333=DIRECTION('',(0.,1.,-2.22044604925031E-16));
#16334=DIRECTION('',(1.,0.,0.));
#16335=DIRECTION('',(0.,1.,-2.22044604925031E-16));
#16336=DIRECTION('',(1.,0.,0.));
#16337=DIRECTION('',(0.,1.,-2.22044604925031E-16));
#16338=DIRECTION('',(1.,0.,0.));
#16339=CARTESIAN_POINT('',(0.,0.,0.));
#16340=CARTESIAN_POINT('',(0.,0.,0.));
#16341=CARTESIAN_POINT('Origin',(2.71767766952966,0.,0.0873223304703366));
#16342=CARTESIAN_POINT('',(2.72071067811865,2.54071067811865,0.0800000000000001));
#16343=CARTESIAN_POINT('',(2.73535533905933,2.52,0.0446446609406728));
#16344=CARTESIAN_POINT('',(2.92352004688311,2.25389491823563,-0.409625128647481));
#16345=CARTESIAN_POINT('',(2.73535533905933,-2.52,0.0446446609406728));
#16346=CARTESIAN_POINT('',(2.73535533905933,0.,0.0446446609406729));
#16347=CARTESIAN_POINT('',(2.72071067811865,-2.54071067811865,0.0800000000000001));
#16348=CARTESIAN_POINT('',(2.93898922848989,-2.23201819180851,-0.446971036681382));
#16349=CARTESIAN_POINT('',(2.7,-2.52,0.13));
#16350=CARTESIAN_POINT('',(2.23461061779379,-2.05461061779379,1.25354935830668));
#16351=CARTESIAN_POINT('',(2.7,2.52,0.13));
#16352=CARTESIAN_POINT('',(2.7,0.,0.13));
#16353=CARTESIAN_POINT('',(2.23461061779379,2.05461061779379,1.25354935830668));
#16354=CARTESIAN_POINT('Origin',(2.7,0.,0.));
#16355=CARTESIAN_POINT('',(2.7,-2.52,5.36678788880707));
#16356=CARTESIAN_POINT('',(2.7,-2.52,2.1875));
#16357=CARTESIAN_POINT('',(2.7,-2.2,5.3));
#16358=CARTESIAN_POINT('Origin',(2.7,-2.2,6.1));
#16359=CARTESIAN_POINT('',(2.7,2.2,5.3));
#16360=CARTESIAN_POINT('',(2.7,0.,5.3));
#16361=CARTESIAN_POINT('',(2.7,2.52,5.36678788880707));
#16362=CARTESIAN_POINT('Origin',(2.7,2.2,6.1));
#16363=CARTESIAN_POINT('',(2.7,2.52,2.1875));
#16364=CARTESIAN_POINT('',(2.7,1.65327317884893E-16,1.65));
#16365=CARTESIAN_POINT('Origin',(2.7,0.,3.));
#16366=CARTESIAN_POINT('Origin',(2.74,-2.56,2.1875));
#16367=CARTESIAN_POINT('',(2.74464466094067,-2.56464466094067,0.0800000000000001));
#16368=CARTESIAN_POINT('',(2.7,-2.52,0.0800000000000001));
#16369=CARTESIAN_POINT('',(2.74464466094067,-2.56464466094067,5.36678788880707));
#16370=CARTESIAN_POINT('',(2.74464466094067,-2.56464466094067,3.28125));
#16371=CARTESIAN_POINT('',(2.78,-2.6,5.36678788880707));
#16372=CARTESIAN_POINT('Origin',(2.78,-2.52,0.));
#16373=CARTESIAN_POINT('',(2.74464466094067,-2.52,0.0353553390593272));
#16374=CARTESIAN_POINT('',(2.78,-2.52,0.));
#16375=CARTESIAN_POINT('',(2.78,-2.54071067811865,0.0207106781186547));
#16376=CARTESIAN_POINT('',(2.29037487135252,-2.25389491823563,0.223520046883111));
#16377=CARTESIAN_POINT('',(2.78,-2.56464466094067,0.0446446609406727));
#16378=CARTESIAN_POINT('',(2.78,-2.6,0.0800000000000001));
#16379=CARTESIAN_POINT('',(2.76693980625181,-2.57387961250363,0.0669398062518134));
#16380=CARTESIAN_POINT('',(2.63047465709621,-2.67037504486719,0.299900387770978));
#16381=CARTESIAN_POINT('',(2.1631759401255,-2.32379243068329,0.420616490557792));
#16382=CARTESIAN_POINT('Origin',(2.78732233047034,0.,0.0176776695296635));
#16383=CARTESIAN_POINT('',(2.74464466094067,2.52,0.0353553390593272));
#16384=CARTESIAN_POINT('',(2.74464466094067,0.,0.0353553390593271));
#16385=CARTESIAN_POINT('',(2.78,2.54071067811865,0.0207106781186547));
#16386=CARTESIAN_POINT('',(2.25302896331862,2.23201819180851,0.238989228489892));
#16387=CARTESIAN_POINT('',(2.83,2.52,0.));
#16388=CARTESIAN_POINT('',(3.20437526486246,2.36492868787695,-0.155071312123047));
#16389=CARTESIAN_POINT('',(2.83,-2.52,0.));
#16390=CARTESIAN_POINT('',(2.83,0.,0.));
#16391=CARTESIAN_POINT('',(3.20437526486246,-2.36492868787695,-0.155071312123047));
#16392=CARTESIAN_POINT('Origin',(5.75,0.,0.));
#16393=CARTESIAN_POINT('',(5.62,2.52,0.));
#16394=CARTESIAN_POINT('',(2.875,2.52,0.));
#16395=CARTESIAN_POINT('',(5.62,-2.52,0.));
#16396=CARTESIAN_POINT('',(5.62,0.,0.));
#16397=CARTESIAN_POINT('',(2.875,-2.52,0.));
#16398=CARTESIAN_POINT('Origin',(2.875,2.56,0.04));
#16399=CARTESIAN_POINT('',(2.78,2.56464466094067,0.0446446609406727));
#16400=CARTESIAN_POINT('',(2.78,2.52,0.));
#16401=CARTESIAN_POINT('',(5.67,2.56464466094067,0.0446446609406727));
#16402=CARTESIAN_POINT('',(1.4375,2.56464466094067,0.0446446609406726));
#16403=CARTESIAN_POINT('',(5.67,2.54071067811865,0.0207106781186545));
#16404=CARTESIAN_POINT('',(5.67,2.6,0.0800000000000001));
#16405=CARTESIAN_POINT('',(4.24052160356021,1.94860133919395,-0.571398660806053));
#16406=CARTESIAN_POINT('Origin',(2.7,2.52,0.08));
#16407=CARTESIAN_POINT('',(2.74464466094067,2.56464466094067,0.0800000000000001));
#16408=CARTESIAN_POINT('',(2.78,2.6,0.0800000000000001));
#16409=CARTESIAN_POINT('',(2.76693980625181,2.57387961250363,0.0669398062518132));
#16410=CARTESIAN_POINT('',(2.12129921369838,2.30644652264939,0.445147308951012));
#16411=CARTESIAN_POINT('',(2.60594383870299,2.68772095290109,0.3417771141981));
#16412=CARTESIAN_POINT('',(2.7,2.52,0.08));
#16413=CARTESIAN_POINT('Origin',(5.66267766952966,0.,0.0176776695296637));
#16414=CARTESIAN_POINT('',(5.70535533905933,2.52,0.0353553390593273));
#16415=CARTESIAN_POINT('',(6.15962512864748,2.25389491823563,0.223520046883112));
#16416=CARTESIAN_POINT('',(5.70535533905933,-2.52,0.0353553390593273));
#16417=CARTESIAN_POINT('',(5.70535533905933,0.,0.0353553390593273));
#16418=CARTESIAN_POINT('',(5.67,-2.54071067811865,0.0207106781186545));
#16419=CARTESIAN_POINT('',(6.19697103668138,-2.23201819180851,0.238989228489893));
#16420=CARTESIAN_POINT('',(4.24052160356021,-1.94860133919395,-0.571398660806053));
#16421=CARTESIAN_POINT('Origin',(2.875,-2.56,0.04));
#16422=CARTESIAN_POINT('',(5.67,-2.56464466094067,0.0446446609406727));
#16423=CARTESIAN_POINT('',(5.67,-2.52,0.));
#16424=CARTESIAN_POINT('',(1.4375,-2.56464466094067,0.0446446609406726));
#16425=CARTESIAN_POINT('Origin',(5.75,-2.52,0.0800000000000001));
#16426=CARTESIAN_POINT('',(5.71464466094067,-2.52,0.0446446609406718));
#16427=CARTESIAN_POINT('',(5.75,-2.52,0.0800000000000001));
#16428=CARTESIAN_POINT('',(5.72928932188135,-2.54071067811866,0.0800000000000001));
#16429=CARTESIAN_POINT('',(5.52647995311688,-2.25389491823565,-0.409625128647469));
#16430=CARTESIAN_POINT('',(5.70535533905933,-2.56464466094067,0.0800000000000001));
#16431=CARTESIAN_POINT('',(5.67,-2.6,0.0800000000000001));
#16432=CARTESIAN_POINT('',(5.68306019374819,-2.57387961250363,0.0669398062518129));
#16433=CARTESIAN_POINT('',(6.75168622086201,-2.1312402189682,0.692926439830206));
#16434=CARTESIAN_POINT('',(5.21257334774201,-2.24119517323359,-0.736231479024399));
#16435=CARTESIAN_POINT('Origin',(5.73232233047034,0.,0.0873223304703347));
#16436=CARTESIAN_POINT('',(5.71464466094067,2.52,0.0446446609406718));
#16437=CARTESIAN_POINT('',(5.71464466094067,0.,0.0446446609406716));
#16438=CARTESIAN_POINT('',(5.72928932188135,2.54071067811866,0.0800000000000001));
#16439=CARTESIAN_POINT('',(5.5110107715101,2.23201819180853,-0.446971036681371));
#16440=CARTESIAN_POINT('',(5.75,2.52,0.129999999999997));
#16441=CARTESIAN_POINT('',(6.88999388238703,1.38000611761297,2.88218869188102));
#16442=CARTESIAN_POINT('',(5.75,-2.52,0.129999999999997));
#16443=CARTESIAN_POINT('',(5.75,0.,0.129999999999998));
#16444=CARTESIAN_POINT('',(6.88999388238703,-1.38000611761297,2.88218869188102));
#16445=CARTESIAN_POINT('Origin',(5.75,0.,8.75));
#16446=CARTESIAN_POINT('',(5.75,2.52,8.62));
#16447=CARTESIAN_POINT('',(5.75,2.52,6.5625));
#16448=CARTESIAN_POINT('',(5.75,-2.52,8.62));
#16449=CARTESIAN_POINT('',(5.75,0.,8.62));
#16450=CARTESIAN_POINT('',(5.75,-2.52,6.5625));
#16451=CARTESIAN_POINT('',(5.75,-1.65327317884893E-16,1.65));
#16452=CARTESIAN_POINT('Origin',(5.75,0.,3.));
#16453=CARTESIAN_POINT('Origin',(5.71,2.56,6.5625));
#16454=CARTESIAN_POINT('',(5.70535533905933,2.56464466094067,0.0800000000000001));
#16455=CARTESIAN_POINT('',(5.75,2.52,0.0800000000000001));
#16456=CARTESIAN_POINT('',(5.70535533905933,2.56464466094067,8.67));
#16457=CARTESIAN_POINT('',(5.70535533905933,2.56464466094067,5.46875));
#16458=CARTESIAN_POINT('',(5.72928932188134,2.54071067811866,8.67));
#16459=CARTESIAN_POINT('',(5.67,2.6,8.67));
#16460=CARTESIAN_POINT('',(6.21538938220622,2.05461061779378,7.49645064169333));
#16461=CARTESIAN_POINT('Origin',(5.67,2.52,0.));
#16462=CARTESIAN_POINT('',(5.68306019374819,2.57387961250363,0.0669398062518126));
#16463=CARTESIAN_POINT('',(5.18804252934879,2.22384926519969,-0.77810820545152));
#16464=CARTESIAN_POINT('',(6.70980949443489,2.1485861270021,0.668395621436986));
#16465=CARTESIAN_POINT('',(5.67,2.52,0.));
#16466=CARTESIAN_POINT('Origin',(5.73232233047034,0.,8.66267766952966));
#16467=CARTESIAN_POINT('',(5.71464466094067,2.52,8.70535533905933));
#16468=CARTESIAN_POINT('',(5.52647995311688,2.25389491823563,9.15962512864748));
#16469=CARTESIAN_POINT('',(5.71464466094067,-2.52,8.70535533905933));
#16470=CARTESIAN_POINT('',(5.71464466094067,0.,8.70535533905933));
#16471=CARTESIAN_POINT('',(5.72928932188134,-2.54071067811866,8.67));
#16472=CARTESIAN_POINT('',(5.5110107715101,-2.23201819180851,9.19697103668138));
#16473=CARTESIAN_POINT('',(6.21538938220622,-2.05461061779378,7.49645064169333));
#16474=CARTESIAN_POINT('Origin',(5.71,-2.56,6.5625));
#16475=CARTESIAN_POINT('',(5.70535533905933,-2.56464466094067,8.67));
#16476=CARTESIAN_POINT('',(5.75,-2.52,8.67));
#16477=CARTESIAN_POINT('',(5.70535533905933,-2.56464466094067,5.46875));
#16478=CARTESIAN_POINT('Origin',(5.67,-2.52,8.75));
#16479=CARTESIAN_POINT('',(5.70535533905933,-2.52,8.71464466094067));
#16480=CARTESIAN_POINT('',(5.67,-2.52,8.75));
#16481=CARTESIAN_POINT('',(5.67,-2.54071067811866,8.72928932188134));
#16482=CARTESIAN_POINT('',(6.15962512864747,-2.25389491823565,8.52647995311689));
#16483=CARTESIAN_POINT('',(5.67,-2.56464466094067,8.70535533905933));
#16484=CARTESIAN_POINT('',(5.67,-2.6,8.67));
#16485=CARTESIAN_POINT('',(5.68306019374819,-2.57387961250363,8.68306019374819));
#16486=CARTESIAN_POINT('',(4.8623899573361,-1.99357812321868,10.0840319194452));
#16487=CARTESIAN_POINT('',(6.28682405987448,-2.3237924306833,8.32938350944224));
#16488=CARTESIAN_POINT('Origin',(5.71,0.,8.71));
#16489=CARTESIAN_POINT('',(5.70535533905933,2.52,8.71464466094067));
#16490=CARTESIAN_POINT('',(5.75,2.52,8.67));
#16491=CARTESIAN_POINT('',(5.70535533905933,0.,8.71464466094067));
#16492=CARTESIAN_POINT('Origin',(5.66267766952966,0.,8.73232233047034));
#16493=CARTESIAN_POINT('',(5.67,2.54071067811866,8.72928932188134));
#16494=CARTESIAN_POINT('',(6.19697103668137,2.23201819180853,8.51101077151011));
#16495=CARTESIAN_POINT('',(5.62,2.52,8.75));
#16496=CARTESIAN_POINT('',(2.10002419371957,1.06197828181349,10.2080217181865));
#16497=CARTESIAN_POINT('',(5.62,-2.52,8.75));
#16498=CARTESIAN_POINT('',(5.62,0.,8.75));
#16499=CARTESIAN_POINT('',(2.10002419371957,-1.06197828181349,10.2080217181865));
#16500=CARTESIAN_POINT('Origin',(-2.875,-2.56,8.71));
#16501=CARTESIAN_POINT('',(-5.62,-2.52,8.75));
#16502=CARTESIAN_POINT('',(-2.875,-2.52,8.75));
#16503=CARTESIAN_POINT('',(-5.67,-2.54071067811865,8.72928932188134));
#16504=CARTESIAN_POINT('',(-4.24052160356022,-1.94860133919393,9.32139866080608));
#16505=CARTESIAN_POINT('',(-5.67,-2.56464466094067,8.70535533905933));
#16506=CARTESIAN_POINT('',(-5.67,-2.52,8.75));
#16507=CARTESIAN_POINT('',(-1.4375,-2.56464466094067,8.70535533905933));
#16508=CARTESIAN_POINT('Origin',(-5.73232233047034,0.,8.66267766952966));
#16509=CARTESIAN_POINT('',(-5.72928932188135,-2.54071067811865,8.67));
#16510=CARTESIAN_POINT('',(-5.71464466094067,-2.52,8.70535533905933));
#16511=CARTESIAN_POINT('',(-5.52647995311689,-2.25389491823563,9.15962512864748));
#16512=CARTESIAN_POINT('',(-5.71464466094067,2.52,8.70535533905933));
#16513=CARTESIAN_POINT('',(-5.71464466094067,0.,8.70535533905933));
#16514=CARTESIAN_POINT('',(-5.72928932188135,2.54071067811865,8.67));
#16515=CARTESIAN_POINT('',(-5.51101077151011,2.23201819180851,9.19697103668138));
#16516=CARTESIAN_POINT('',(-5.75,2.52,8.62));
#16517=CARTESIAN_POINT('',(-6.889993882387,1.380006117613,5.86781130811893));
#16518=CARTESIAN_POINT('',(-5.75,-2.52,8.62));
#16519=CARTESIAN_POINT('',(-5.75,0.,8.62));
#16520=CARTESIAN_POINT('',(-6.889993882387,-1.380006117613,5.86781130811893));
#16521=CARTESIAN_POINT('Origin',(-5.75,-2.52,8.67));
#16522=CARTESIAN_POINT('',(-5.70535533905933,-2.56464466094067,8.67));
#16523=CARTESIAN_POINT('',(-5.67,-2.6,8.67));
#16524=CARTESIAN_POINT('',(-5.68306019374819,-2.57387961250363,8.68306019374819));
#16525=CARTESIAN_POINT('',(-6.75168622086201,-2.1312402189682,8.05707356016979));
#16526=CARTESIAN_POINT('',(-5.21257334774201,-2.24119517323359,9.4862314790244));
#16527=CARTESIAN_POINT('',(-5.70535533905933,-2.52,8.71464466094067));
#16528=CARTESIAN_POINT('',(-6.19697103668137,-2.23201819180853,8.5110107715101));
#16529=CARTESIAN_POINT('',(-5.75,-2.52,8.67));
#16530=CARTESIAN_POINT('Origin',(-5.71,-2.56,2.1875));
#16531=CARTESIAN_POINT('',(-5.75,-2.52,0.129999999999999));
#16532=CARTESIAN_POINT('',(-5.75,-2.52,2.1875));
#16533=CARTESIAN_POINT('',(-5.72928932188135,-2.54071067811865,0.0800000000000001));
#16534=CARTESIAN_POINT('',(-6.21538938220622,-2.05461061779379,1.25354935830668));
#16535=CARTESIAN_POINT('',(-5.70535533905933,-2.56464466094067,0.0800000000000001));
#16536=CARTESIAN_POINT('',(-5.75,-2.52,0.0800000000000001));
#16537=CARTESIAN_POINT('',(-5.70535533905933,-2.56464466094067,3.28125));
#16538=CARTESIAN_POINT('Origin',(-5.75,0.,0.));
#16539=CARTESIAN_POINT('',(-5.75,2.52,0.129999999999999));
#16540=CARTESIAN_POINT('',(-5.75,2.52,2.1875));
#16541=CARTESIAN_POINT('',(-5.75,0.,0.129999999999999));
#16542=CARTESIAN_POINT('',(-5.75,1.65327317884893E-16,1.65));
#16543=CARTESIAN_POINT('Origin',(-5.75,0.,3.));
#16544=CARTESIAN_POINT('Origin',(-5.66267766952967,0.,8.73232233047034));
#16545=CARTESIAN_POINT('',(-5.67,2.54071067811865,8.72928932188134));
#16546=CARTESIAN_POINT('',(-5.70535533905933,2.52,8.71464466094067));
#16547=CARTESIAN_POINT('',(-6.15962512864747,2.25389491823565,8.52647995311688));
#16548=CARTESIAN_POINT('',(-5.70535533905933,0.,8.71464466094067));
#16549=CARTESIAN_POINT('',(-5.62,2.52,8.75));
#16550=CARTESIAN_POINT('',(-5.62,0.,8.75));
#16551=CARTESIAN_POINT('',(-4.24052160356022,1.94860133919393,9.32139866080608));
#16552=CARTESIAN_POINT('Origin',(-5.71,0.,8.71));
#16553=CARTESIAN_POINT('',(-5.67,2.52,8.75));
#16554=CARTESIAN_POINT('Origin',(-5.67,2.52,8.75));
#16555=CARTESIAN_POINT('',(-5.67,2.56464466094067,8.70535533905933));
#16556=CARTESIAN_POINT('',(-5.67,2.6,8.67));
#16557=CARTESIAN_POINT('',(-5.68306019374819,2.57387961250363,8.68306019374819));
#16558=CARTESIAN_POINT('',(-5.18804252934879,2.22384926519969,9.52810820545152));
#16559=CARTESIAN_POINT('',(-5.70535533905933,2.56464466094067,8.67));
#16560=CARTESIAN_POINT('',(-6.70980949443489,2.1485861270021,8.08160437856301));
#16561=CARTESIAN_POINT('',(-5.75,2.52,8.67));
#16562=CARTESIAN_POINT('Origin',(-2.875,2.56,8.71));
#16563=CARTESIAN_POINT('',(5.67,2.56464466094067,8.70535533905933));
#16564=CARTESIAN_POINT('',(5.67,2.52,8.75));
#16565=CARTESIAN_POINT('',(-1.4375,2.56464466094067,8.70535533905933));
#16566=CARTESIAN_POINT('',(-2.875,2.52,8.75));
#16567=CARTESIAN_POINT('Origin',(-5.73232233047034,0.,0.0873223304703359));
#16568=CARTESIAN_POINT('',(-5.72928932188135,2.54071067811865,0.0800000000000001));
#16569=CARTESIAN_POINT('',(-5.71464466094067,2.52,0.0446446609406726));
#16570=CARTESIAN_POINT('',(-5.52647995311689,2.25389491823563,-0.409625128647479));
#16571=CARTESIAN_POINT('',(-5.71464466094067,-2.52,0.0446446609406726));
#16572=CARTESIAN_POINT('',(-5.71464466094067,0.,0.0446446609406725));
#16573=CARTESIAN_POINT('',(-5.51101077151011,-2.23201819180851,-0.44697103668138));
#16574=CARTESIAN_POINT('',(-6.21538938220622,2.05461061779379,1.25354935830668));
#16575=CARTESIAN_POINT('Origin',(-5.67,-2.52,0.));
#16576=CARTESIAN_POINT('',(-5.70535533905933,-2.52,0.035355339059328));
#16577=CARTESIAN_POINT('',(-5.67,-2.52,0.));
#16578=CARTESIAN_POINT('',(-5.67,-2.54071067811865,0.0207106781186548));
#16579=CARTESIAN_POINT('',(-6.15962512864748,-2.25389491823564,0.223520046883113));
#16580=CARTESIAN_POINT('',(-5.67,-2.56464466094067,0.0446446609406727));
#16581=CARTESIAN_POINT('',(-5.67,-2.6,0.0800000000000001));
#16582=CARTESIAN_POINT('',(-5.68306019374819,-2.57387961250363,0.0669398062518126));
#16583=CARTESIAN_POINT('',(-5.10167380372804,-2.16277735363081,-0.925548842641145));
#16584=CARTESIAN_POINT('',(-6.28682405987449,-2.32379243068329,0.420616490557785));
#16585=CARTESIAN_POINT('Origin',(-5.66267766952966,0.,0.0176776695296639));
#16586=CARTESIAN_POINT('',(-5.70535533905933,2.52,0.035355339059328));
#16587=CARTESIAN_POINT('',(-5.70535533905933,0.,0.0353553390593278));
#16588=CARTESIAN_POINT('',(-5.67,2.54071067811865,0.0207106781186548));
#16589=CARTESIAN_POINT('',(-6.19697103668138,2.23201819180852,0.238989228489894));
#16590=CARTESIAN_POINT('',(-5.62,2.52,0.));
#16591=CARTESIAN_POINT('',(-3.67282446442857,1.71345348484521,-0.806546515154792));
#16592=CARTESIAN_POINT('',(-5.62,-2.52,0.));
#16593=CARTESIAN_POINT('',(-5.62,0.,0.));
#16594=CARTESIAN_POINT('',(-3.67282446442857,-1.71345348484521,-0.806546515154792));
#16595=CARTESIAN_POINT('Origin',(-2.7,0.,0.));
#16596=CARTESIAN_POINT('',(-2.83,2.52,0.));
#16597=CARTESIAN_POINT('',(-1.35,2.52,0.));
#16598=CARTESIAN_POINT('',(-2.83,-2.52,0.));
#16599=CARTESIAN_POINT('',(-2.83,0.,0.));
#16600=CARTESIAN_POINT('',(-1.35,-2.52,0.));
#16601=CARTESIAN_POINT('Origin',(-1.35,2.56,0.04));
#16602=CARTESIAN_POINT('',(-5.67,2.56464466094067,0.0446446609406727));
#16603=CARTESIAN_POINT('',(-5.67,2.52,0.));
#16604=CARTESIAN_POINT('',(-2.78,2.56464466094067,0.0446446609406727));
#16605=CARTESIAN_POINT('',(-0.675,2.56464466094067,0.0446446609406726));
#16606=CARTESIAN_POINT('',(-2.78,2.54071067811865,0.0207106781186546));
#16607=CARTESIAN_POINT('',(-2.78,2.6,0.0800000000000001));
#16608=CARTESIAN_POINT('',(-2.63667812573082,2.60007654222568,0.0800765422256816));
#16609=CARTESIAN_POINT('Origin',(-5.75,2.52,0.08));
#16610=CARTESIAN_POINT('',(-5.70535533905933,2.56464466094067,0.0800000000000001));
#16611=CARTESIAN_POINT('',(-5.67,2.6,0.0800000000000001));
#16612=CARTESIAN_POINT('',(-5.68306019374819,2.57387961250363,0.0669398062518126));
#16613=CARTESIAN_POINT('',(-6.32870078630161,2.30644652264939,0.445147308951005));
#16614=CARTESIAN_POINT('',(-5.12620462212126,2.18012326166471,-0.883672116214024));
#16615=CARTESIAN_POINT('',(-5.75,2.52,0.08));
#16616=CARTESIAN_POINT('Origin',(-2.78732233047034,0.,0.0176776695296638));
#16617=CARTESIAN_POINT('',(-2.74464466094067,2.52,0.0353553390593276));
#16618=CARTESIAN_POINT('',(-2.29037487135252,2.25389491823563,0.223520046883113));
#16619=CARTESIAN_POINT('',(-2.74464466094067,-2.52,0.0353553390593277));
#16620=CARTESIAN_POINT('',(-2.74464466094067,0.,0.0353553390593275));
#16621=CARTESIAN_POINT('',(-2.78,-2.54071067811865,0.0207106781186546));
#16622=CARTESIAN_POINT('',(-2.25302896331862,-2.23201819180851,0.238989228489893));
#16623=CARTESIAN_POINT('',(-2.63667812573082,-2.60007654222568,0.0800765422256816));
#16624=CARTESIAN_POINT('Origin',(-1.35,-2.56,0.04));
#16625=CARTESIAN_POINT('',(-2.78,-2.56464466094067,0.0446446609406727));
#16626=CARTESIAN_POINT('',(-2.78,-2.52,0.));
#16627=CARTESIAN_POINT('',(-0.675,-2.56464466094067,0.0446446609406726));
#16628=CARTESIAN_POINT('Origin',(-2.7,-2.52,0.0800000000000001));
#16629=CARTESIAN_POINT('',(-2.73535533905933,-2.52,0.0446446609406727));
#16630=CARTESIAN_POINT('',(-2.7,-2.52,0.0800000000000001));
#16631=CARTESIAN_POINT('',(-2.72071067811865,-2.54071067811865,0.0800000000000001));
#16632=CARTESIAN_POINT('',(-2.92352004688311,-2.25389491823563,-0.409625128647479));
#16633=CARTESIAN_POINT('',(-2.74464466094067,-2.56464466094067,0.0800000000000001));
#16634=CARTESIAN_POINT('',(-2.78,-2.6,0.0800000000000001));
#16635=CARTESIAN_POINT('',(-2.76693980625181,-2.57387961250363,0.0669398062518135));
#16636=CARTESIAN_POINT('',(-1.84575441632761,-2.19231213053707,0.606557714209465));
#16637=CARTESIAN_POINT('',(-2.51957511308224,-2.74879286446996,0.489217751387724));
#16638=CARTESIAN_POINT('Origin',(-2.71767766952966,0.,0.087322330470336));
#16639=CARTESIAN_POINT('',(-2.73535533905933,2.52,0.0446446609406726));
#16640=CARTESIAN_POINT('',(-2.73535533905933,0.,0.0446446609406725));
#16641=CARTESIAN_POINT('',(-2.72071067811865,2.54071067811865,0.0800000000000001));
#16642=CARTESIAN_POINT('',(-2.93898922848989,2.23201819180851,-0.44697103668138));
#16643=CARTESIAN_POINT('',(-2.7,2.52,0.129999999999999));
#16644=CARTESIAN_POINT('',(-1.79515397196173,1.61515397196173,2.31449155274942));
#16645=CARTESIAN_POINT('',(-2.7,-2.52,0.129999999999999));
#16646=CARTESIAN_POINT('',(-2.7,0.,0.129999999999999));
#16647=CARTESIAN_POINT('',(-1.79515397196173,-1.61515397196173,2.31449155274942));
#16648=CARTESIAN_POINT('Origin',(-2.7,0.,5.7));
#16649=CARTESIAN_POINT('',(-2.7,2.52,5.36678788880707));
#16650=CARTESIAN_POINT('',(-2.7,2.52,5.0375));
#16651=CARTESIAN_POINT('',(-2.7,2.2,5.3));
#16652=CARTESIAN_POINT('Origin',(-2.7,2.2,6.1));
#16653=CARTESIAN_POINT('',(-2.7,-2.2,5.3));
#16654=CARTESIAN_POINT('',(-2.7,0.,5.3));
#16655=CARTESIAN_POINT('',(-2.7,-2.52,5.36678788880707));
#16656=CARTESIAN_POINT('Origin',(-2.7,-2.2,6.1));
#16657=CARTESIAN_POINT('',(-2.7,-2.52,5.0375));
#16658=CARTESIAN_POINT('',(-2.7,-1.65327317884893E-16,1.65));
#16659=CARTESIAN_POINT('Origin',(-2.7,0.,3.));
#16660=CARTESIAN_POINT('Origin',(-2.74,2.56,5.0375));
#16661=CARTESIAN_POINT('',(-2.74464466094067,2.56464466094067,0.0800000000000001));
#16662=CARTESIAN_POINT('',(-2.7,2.52,0.0800000000000001));
#16663=CARTESIAN_POINT('',(-2.74464466094067,2.56464466094067,5.36678788880707));
#16664=CARTESIAN_POINT('',(-2.74464466094067,2.56464466094067,4.70625));
#16665=CARTESIAN_POINT('',(-2.78,2.6,5.36678788880707));
#16666=CARTESIAN_POINT('Origin',(-2.78,2.52,0.));
#16667=CARTESIAN_POINT('',(-2.76693980625181,2.57387961250363,0.0669398062518129));
#16668=CARTESIAN_POINT('',(-2.54410593147546,2.73144695643606,0.447341024960603));
#16669=CARTESIAN_POINT('',(-1.88763114275473,2.20965803857097,0.582026895816245));
#16670=CARTESIAN_POINT('',(-2.78,2.52,0.));
#16671=CARTESIAN_POINT('Origin',(-0.675,-2.58232233047034,0.0873223304703362));
#16672=CARTESIAN_POINT('',(-2.83,-2.6,0.13));
#16673=CARTESIAN_POINT('',(-3.36446283715638,-2.82138175573458,0.664462837156383));
#16674=CARTESIAN_POINT('',(-5.62,-2.6,0.13));
#16675=CARTESIAN_POINT('',(-0.675,-2.6,0.13));
#16676=CARTESIAN_POINT('',(-3.77888057658085,-3.36261663512876,1.97111942341917));
#16677=CARTESIAN_POINT('Origin',(-2.78732233047034,-2.58232233047034,4.70625));
#16678=CARTESIAN_POINT('',(-2.74464466094067,-2.56464466094067,5.36678788880707));
#16679=CARTESIAN_POINT('',(-2.74464466094067,-2.56464466094067,4.70625));
#16680=CARTESIAN_POINT('',(-2.83,-2.6,5.36678788880707));
#16681=CARTESIAN_POINT('',(-2.83,-2.6,5.36678788880707));
#16682=CARTESIAN_POINT('',(-2.83,-2.6,4.70625));
#16683=CARTESIAN_POINT('Ctrl Pts',(-2.74442178368363,-2.56486895213994,
5.39792313687514));
#16684=CARTESIAN_POINT('Ctrl Pts',(-2.74456950540178,-2.56471935013366,
5.38754472085245));
#16685=CARTESIAN_POINT('Ctrl Pts',(-2.74464466094067,-2.56464466094067,
5.37716630482976));
#16686=CARTESIAN_POINT('Ctrl Pts',(-2.74464466094067,-2.56464466094067,
5.36678788880707));
#16687=CARTESIAN_POINT('Ctrl Pts',(-2.77294785578909,-2.57657930142663,
5.39792313687514));
#16688=CARTESIAN_POINT('Ctrl Pts',(-2.77304633693452,-2.57647956675577,
5.38754472085245));
#16689=CARTESIAN_POINT('Ctrl Pts',(-2.77309644062712,-2.57642977396045,
5.37716630482976));
#16690=CARTESIAN_POINT('Ctrl Pts',(-2.77309644062712,-2.57642977396045,
5.36678788880707));
#16691=CARTESIAN_POINT('Ctrl Pts',(-2.80147392789454,-2.58828965071331,
5.39792313687514));
#16692=CARTESIAN_POINT('Ctrl Pts',(-2.80152316846726,-2.58823978337789,
5.38754472085245));
#16693=CARTESIAN_POINT('Ctrl Pts',(-2.80154822031356,-2.58821488698022,
5.37716630482976));
#16694=CARTESIAN_POINT('Ctrl Pts',(-2.80154822031356,-2.58821488698022,
5.36678788880707));
#16695=CARTESIAN_POINT('Ctrl Pts',(-2.83,-2.6,5.39792313687514));
#16696=CARTESIAN_POINT('Ctrl Pts',(-2.83,-2.6,5.38754472085245));
#16697=CARTESIAN_POINT('Ctrl Pts',(-2.83,-2.6,5.37716630482976));
#16698=CARTESIAN_POINT('Ctrl Pts',(-2.83,-2.6,5.36678788880707));
#16699=CARTESIAN_POINT('',(-2.74442178368363,-2.56486895213994,5.39792313687514));
#16700=CARTESIAN_POINT('',(-2.83,-2.6,5.39792313687514));
#16701=CARTESIAN_POINT('Ctrl Pts',(-2.74442178368363,-2.56486895213994,
5.39792313687514));
#16702=CARTESIAN_POINT('Ctrl Pts',(-2.77294785578909,-2.57657930142663,
5.39792313687514));
#16703=CARTESIAN_POINT('Ctrl Pts',(-2.80147392789454,-2.58828965071331,
5.39792313687514));
#16704=CARTESIAN_POINT('Ctrl Pts',(-2.83,-2.6,5.39792313687514));
#16705=CARTESIAN_POINT('Ctrl Pts',(-2.83,-2.6,5.39792313687514));
#16706=CARTESIAN_POINT('Ctrl Pts',(-2.83,-2.6,5.38754472085245));
#16707=CARTESIAN_POINT('Ctrl Pts',(-2.83,-2.6,5.37716630482976));
#16708=CARTESIAN_POINT('Ctrl Pts',(-2.83,-2.6,5.36678788880707));
#16709=CARTESIAN_POINT('Ctrl Pts',(-2.74464466094067,-2.56464466094067,
5.36678788880707));
#16710=CARTESIAN_POINT('Ctrl Pts',(-2.74464466094067,-2.56464466094067,
5.37716630482976));
#16711=CARTESIAN_POINT('Ctrl Pts',(-2.74456950540178,-2.56471935013366,
5.38754472085245));
#16712=CARTESIAN_POINT('Ctrl Pts',(-2.74442178368363,-2.56486895213994,
5.39792313687514));
#16713=CARTESIAN_POINT('Ctrl Pts',(-2.74442178368363,-2.56486895213994,
5.39792313687514));
#16714=CARTESIAN_POINT('Ctrl Pts',(-2.75619335349611,-2.57658041242369,
5.40100865024091));
#16715=CARTESIAN_POINT('Ctrl Pts',(-2.76803982089572,-2.58829135908796,
5.40409416360668));
#16716=CARTESIAN_POINT('Ctrl Pts',(-2.78,-2.6,5.40717967697245));
#16717=CARTESIAN_POINT('Ctrl Pts',(-2.77294785578909,-2.57657930142663,
5.39792313687514));
#16718=CARTESIAN_POINT('Ctrl Pts',(-2.77524001344185,-2.58438694161579,
5.40100865024091));
#16719=CARTESIAN_POINT('Ctrl Pts',(-2.77758210281937,-2.59219423939197,
5.40409416360668));
#16720=CARTESIAN_POINT('Ctrl Pts',(-2.78,-2.6,5.40717967697245));
#16721=CARTESIAN_POINT('Ctrl Pts',(-2.80147392789454,-2.58828965071331,
5.39792313687514));
#16722=CARTESIAN_POINT('Ctrl Pts',(-2.79428667338759,-2.5921934708079,5.40100865024091));
#16723=CARTESIAN_POINT('Ctrl Pts',(-2.78712438474302,-2.59609711969599,
5.40409416360668));
#16724=CARTESIAN_POINT('Ctrl Pts',(-2.78,-2.6,5.40717967697245));
#16725=CARTESIAN_POINT('Ctrl Pts',(-2.83,-2.6,5.39792313687514));
#16726=CARTESIAN_POINT('Ctrl Pts',(-2.81333333333333,-2.6,5.40100865024091));
#16727=CARTESIAN_POINT('Ctrl Pts',(-2.79666666666667,-2.6,5.40409416360668));
#16728=CARTESIAN_POINT('Ctrl Pts',(-2.78,-2.6,5.40717967697245));
#16729=CARTESIAN_POINT('',(-2.78,-2.6,5.40717967697245));
#16730=CARTESIAN_POINT('Ctrl Pts',(-2.74442178368363,-2.56486895213994,
5.39792313687514));
#16731=CARTESIAN_POINT('Ctrl Pts',(-2.75619335349611,-2.57658041242369,
5.40100865024091));
#16732=CARTESIAN_POINT('Ctrl Pts',(-2.76803982089572,-2.58829135908796,
5.40409416360668));
#16733=CARTESIAN_POINT('Ctrl Pts',(-2.78,-2.6,5.40717967697245));
#16734=CARTESIAN_POINT('Ctrl Pts',(-2.78,-2.6,5.40717967697245));
#16735=CARTESIAN_POINT('Ctrl Pts',(-2.79666666666667,-2.6,5.40409416360668));
#16736=CARTESIAN_POINT('Ctrl Pts',(-2.81333333333333,-2.6,5.40100865024091));
#16737=CARTESIAN_POINT('Ctrl Pts',(-2.83,-2.6,5.39792313687514));
#16738=CARTESIAN_POINT('Origin',(0.,-2.6,4.375));
#16739=CARTESIAN_POINT('',(-2.42414283215669,-2.6,6.08851340213307));
#16740=CARTESIAN_POINT('Ctrl Pts',(-2.42414283215669,-2.6,6.08851340213307));
#16741=CARTESIAN_POINT('Ctrl Pts',(-2.47340183676932,-2.6,6.03819996865104));
#16742=CARTESIAN_POINT('Ctrl Pts',(-2.55014714354309,-2.6,5.9563590107329));
#16743=CARTESIAN_POINT('Ctrl Pts',(-2.6396310734963,-2.6,5.83483846916786));
#16744=CARTESIAN_POINT('Ctrl Pts',(-2.69414240597218,-2.6,5.74352625586477));
#16745=CARTESIAN_POINT('Ctrl Pts',(-2.74081734015966,-2.6,5.6395635803662));
#16746=CARTESIAN_POINT('Ctrl Pts',(-2.77299866241655,-2.6,5.52278122462383));
#16747=CARTESIAN_POINT('Ctrl Pts',(-2.78,-2.6,5.44464477671195));
#16748=CARTESIAN_POINT('Ctrl Pts',(-2.78,-2.6,5.40717967697245));
#16749=CARTESIAN_POINT('',(-2.3,-2.6,6.1));
#16750=CARTESIAN_POINT('Ctrl Pts',(-2.3,-2.6,6.1));
#16751=CARTESIAN_POINT('Ctrl Pts',(-2.34138094405223,-2.6,6.09617113404436));
#16752=CARTESIAN_POINT('Ctrl Pts',(-2.38276188810446,-2.6,6.09234226808871));
#16753=CARTESIAN_POINT('Ctrl Pts',(-2.42414283215669,-2.6,6.08851340213307));
#16754=CARTESIAN_POINT('',(2.3,-2.6,6.1));
#16755=CARTESIAN_POINT('',(1.35,-2.6,6.1));
#16756=CARTESIAN_POINT('',(2.42414283239008,-2.6,6.08851340189468));
#16757=CARTESIAN_POINT('Ctrl Pts',(2.42414283239008,-2.6,6.08851340189468));
#16758=CARTESIAN_POINT('Ctrl Pts',(2.38276188826005,-2.6,6.09234226792978));
#16759=CARTESIAN_POINT('Ctrl Pts',(2.34138094413003,-2.6,6.09617113396489));
#16760=CARTESIAN_POINT('Ctrl Pts',(2.3,-2.6,6.1));
#16761=CARTESIAN_POINT('',(2.78,-2.6,5.40717967697245));
#16762=CARTESIAN_POINT('Ctrl Pts',(2.78,-2.6,5.40717967697245));
#16763=CARTESIAN_POINT('Ctrl Pts',(2.78,-2.6,5.44865469871872));
#16764=CARTESIAN_POINT('Ctrl Pts',(2.77175013108469,-2.6,5.53495446115542));
#16765=CARTESIAN_POINT('Ctrl Pts',(2.73152937534889,-2.6,5.66466680090526));
#16766=CARTESIAN_POINT('Ctrl Pts',(2.66093134122623,-2.6,5.80894311125375));
#16767=CARTESIAN_POINT('Ctrl Pts',(2.5873706385557,-2.6,5.90812597923557));
#16768=CARTESIAN_POINT('Ctrl Pts',(2.49738496881261,-2.6,6.0124608445315));
#16769=CARTESIAN_POINT('Ctrl Pts',(2.46022125233207,-2.6,6.05166269416259));
#16770=CARTESIAN_POINT('Ctrl Pts',(2.42414283239008,-2.6,6.08851340189468));
#16771=CARTESIAN_POINT('',(2.83,-2.6,5.39792313665174));
#16772=CARTESIAN_POINT('Ctrl Pts',(2.83,-2.6,5.39792313665174));
#16773=CARTESIAN_POINT('Ctrl Pts',(2.81333333333333,-2.6,5.40100865009198));
#16774=CARTESIAN_POINT('Ctrl Pts',(2.79666666666667,-2.6,5.40409416353221));
#16775=CARTESIAN_POINT('Ctrl Pts',(2.78,-2.6,5.40717967697245));
#16776=CARTESIAN_POINT('',(2.83,-2.6,5.36678788880707));
#16777=CARTESIAN_POINT('Ctrl Pts',(2.83,-2.6,5.36678788880707));
#16778=CARTESIAN_POINT('Ctrl Pts',(2.83,-2.6,5.37716630475529));
#16779=CARTESIAN_POINT('Ctrl Pts',(2.83,-2.6,5.38754472070352));
#16780=CARTESIAN_POINT('Ctrl Pts',(2.83,-2.6,5.39792313665175));
#16781=CARTESIAN_POINT('',(2.83,-2.6,0.13));
#16782=CARTESIAN_POINT('',(2.83,-2.6,3.28125));
#16783=CARTESIAN_POINT('',(5.62,-2.6,0.13));
#16784=CARTESIAN_POINT('',(1.4375,-2.6,0.13));
#16785=CARTESIAN_POINT('',(5.62,-2.6,8.62));
#16786=CARTESIAN_POINT('',(5.62,-2.6,5.46875));
#16787=CARTESIAN_POINT('',(-5.62,-2.6,8.62));
#16788=CARTESIAN_POINT('',(-1.4375,-2.6,8.62));
#16789=CARTESIAN_POINT('',(-5.62,-2.6,3.28125));
#16790=CARTESIAN_POINT('',(4.21,-2.6,1.));
#16791=CARTESIAN_POINT('Origin',(4.6,-2.6,1.));
#16792=CARTESIAN_POINT('',(-4.99,-2.6,1.));
#16793=CARTESIAN_POINT('Origin',(-4.6,-2.6,1.));
#16794=CARTESIAN_POINT('',(4.21,-2.6,7.75));
#16795=CARTESIAN_POINT('Origin',(4.6,-2.6,7.75));
#16796=CARTESIAN_POINT('',(-4.99,-2.6,7.75));
#16797=CARTESIAN_POINT('Origin',(-4.6,-2.6,7.75));
#16798=CARTESIAN_POINT('Ctrl Pts',(-2.69829980684391,-2.52001806864527,
5.40717967697245));
#16799=CARTESIAN_POINT('Ctrl Pts',(-2.69942945076934,-2.51999405556084,
5.39371574758399));
#16800=CARTESIAN_POINT('Ctrl Pts',(-2.7,-2.52,5.38025181819553));
#16801=CARTESIAN_POINT('Ctrl Pts',(-2.7,-2.52,5.36678788880707));
#16802=CARTESIAN_POINT('Ctrl Pts',(-2.7255332045626,-2.54667871243018,5.40717967697245));
#16803=CARTESIAN_POINT('Ctrl Pts',(-2.72628630051289,-2.54666270370723,
5.39371574758399));
#16804=CARTESIAN_POINT('Ctrl Pts',(-2.72666666666667,-2.54666666666667,
5.38025181819553));
#16805=CARTESIAN_POINT('Ctrl Pts',(-2.72666666666667,-2.54666666666667,
5.36678788880707));
#16806=CARTESIAN_POINT('Ctrl Pts',(-2.7527666022813,-2.57333935621509,5.40717967697245));
#16807=CARTESIAN_POINT('Ctrl Pts',(-2.75314315025645,-2.57333135185361,
5.39371574758399));
#16808=CARTESIAN_POINT('Ctrl Pts',(-2.75333333333333,-2.57333333333333,
5.38025181819553));
#16809=CARTESIAN_POINT('Ctrl Pts',(-2.75333333333333,-2.57333333333333,
5.36678788880707));
#16810=CARTESIAN_POINT('Ctrl Pts',(-2.78,-2.6,5.40717967697245));
#16811=CARTESIAN_POINT('Ctrl Pts',(-2.78,-2.6,5.39371574758399));
#16812=CARTESIAN_POINT('Ctrl Pts',(-2.78,-2.6,5.38025181819553));
#16813=CARTESIAN_POINT('Ctrl Pts',(-2.78,-2.6,5.36678788880707));
#16814=CARTESIAN_POINT('',(-2.7,-2.52,5.36678788880707));
#16815=CARTESIAN_POINT('',(-2.69829980684391,-2.52001806864527,5.40717967697245));
#16816=CARTESIAN_POINT('Ctrl Pts',(-2.7,-2.52,5.36678788880707));
#16817=CARTESIAN_POINT('Ctrl Pts',(-2.7,-2.52,5.38025181819553));
#16818=CARTESIAN_POINT('Ctrl Pts',(-2.69942945076934,-2.51999405556084,
5.39371574758399));
#16819=CARTESIAN_POINT('Ctrl Pts',(-2.69829980684391,-2.52001806864527,
5.40717967697245));
#16820=CARTESIAN_POINT('',(-2.78,-2.6,5.40717967697245));
#16821=CARTESIAN_POINT('Origin',(-1.4375,-2.58232233047034,8.66267766952966));
#16822=CARTESIAN_POINT('',(-3.45077738091134,-3.49852142863302,6.45077738091131));
#16823=CARTESIAN_POINT('',(3.29248197949184,-3.56408953076227,6.29248197949182));
#16824=CARTESIAN_POINT('Origin',(-5.66267766952966,-2.58232233047034,3.28125));
#16825=CARTESIAN_POINT('Origin',(1.4375,-2.58232233047034,0.0873223304703362));
#16826=CARTESIAN_POINT('',(3.45077738091134,-3.49852142863302,2.29922261908869));
#16827=CARTESIAN_POINT('',(3.21192363215214,-2.75819794822821,0.511923632152139));
#16828=CARTESIAN_POINT('Origin',(5.66267766952966,-2.58232233047034,5.46875));
#16829=CARTESIAN_POINT('Origin',(2.78732233047034,-2.58232233047034,3.28125));
#16830=CARTESIAN_POINT('',(2.83,-2.6,5.36678788880707));
#16831=CARTESIAN_POINT('Ctrl Pts',(2.74464466094067,-2.56464466094067,5.36678788880707));
#16832=CARTESIAN_POINT('Ctrl Pts',(2.74464466094067,-2.56464466094067,5.37716630475529));
#16833=CARTESIAN_POINT('Ctrl Pts',(2.74456950540286,-2.56471935013259,5.38754472070352));
#16834=CARTESIAN_POINT('Ctrl Pts',(2.74442178368681,-2.56486895213672,5.39792313665175));
#16835=CARTESIAN_POINT('Ctrl Pts',(2.77309644062712,-2.57642977396045,5.36678788880707));
#16836=CARTESIAN_POINT('Ctrl Pts',(2.77309644062712,-2.57642977396045,5.37716630475529));
#16837=CARTESIAN_POINT('Ctrl Pts',(2.77304633693524,-2.57647956675506,5.38754472070352));
#16838=CARTESIAN_POINT('Ctrl Pts',(2.77294785579121,-2.57657930142448,5.39792313665175));
#16839=CARTESIAN_POINT('Ctrl Pts',(2.80154822031356,-2.58821488698022,5.36678788880707));
#16840=CARTESIAN_POINT('Ctrl Pts',(2.80154822031356,-2.58821488698022,5.37716630475529));
#16841=CARTESIAN_POINT('Ctrl Pts',(2.80152316846762,-2.58823978337753,5.38754472070352));
#16842=CARTESIAN_POINT('Ctrl Pts',(2.8014739278956,-2.58828965071224,5.39792313665175));
#16843=CARTESIAN_POINT('Ctrl Pts',(2.83,-2.6,5.36678788880707));
#16844=CARTESIAN_POINT('Ctrl Pts',(2.83,-2.6,5.37716630475529));
#16845=CARTESIAN_POINT('Ctrl Pts',(2.83,-2.6,5.38754472070352));
#16846=CARTESIAN_POINT('Ctrl Pts',(2.83,-2.6,5.39792313665175));
#16847=CARTESIAN_POINT('',(2.74442178368681,-2.56486895213672,5.39792313665174));
#16848=CARTESIAN_POINT('Ctrl Pts',(2.83,-2.6,5.39792313665175));
#16849=CARTESIAN_POINT('Ctrl Pts',(2.8014739278956,-2.58828965071224,5.39792313665175));
#16850=CARTESIAN_POINT('Ctrl Pts',(2.77294785579121,-2.57657930142448,5.39792313665175));
#16851=CARTESIAN_POINT('Ctrl Pts',(2.74442178368681,-2.56486895213672,5.39792313665175));
#16852=CARTESIAN_POINT('Ctrl Pts',(2.74442178368681,-2.56486895213672,5.39792313665175));
#16853=CARTESIAN_POINT('Ctrl Pts',(2.74456950540286,-2.56471935013259,5.38754472070352));
#16854=CARTESIAN_POINT('Ctrl Pts',(2.74464466094067,-2.56464466094067,5.37716630475529));
#16855=CARTESIAN_POINT('Ctrl Pts',(2.74464466094067,-2.56464466094067,5.36678788880707));
#16856=CARTESIAN_POINT('Ctrl Pts',(2.83,-2.6,5.39792313665174));
#16857=CARTESIAN_POINT('Ctrl Pts',(2.81333333333333,-2.6,5.40100865009198));
#16858=CARTESIAN_POINT('Ctrl Pts',(2.79666666666667,-2.6,5.40409416353221));
#16859=CARTESIAN_POINT('Ctrl Pts',(2.78,-2.6,5.40717967697245));
#16860=CARTESIAN_POINT('Ctrl Pts',(2.8014739278956,-2.58828965071224,5.39792313665174));
#16861=CARTESIAN_POINT('Ctrl Pts',(2.7942866733878,-2.59219347080718,5.40100865009198));
#16862=CARTESIAN_POINT('Ctrl Pts',(2.78712438474266,-2.59609711969564,5.40409416353221));
#16863=CARTESIAN_POINT('Ctrl Pts',(2.78,-2.6,5.40717967697245));
#16864=CARTESIAN_POINT('Ctrl Pts',(2.77294785579121,-2.57657930142448,5.39792313665174));
#16865=CARTESIAN_POINT('Ctrl Pts',(2.77524001344226,-2.58438694161436,5.40100865009198));
#16866=CARTESIAN_POINT('Ctrl Pts',(2.77758210281866,-2.59219423939128,5.40409416353221));
#16867=CARTESIAN_POINT('Ctrl Pts',(2.78,-2.6,5.40717967697245));
#16868=CARTESIAN_POINT('Ctrl Pts',(2.74442178368681,-2.56486895213672,5.39792313665174));
#16869=CARTESIAN_POINT('Ctrl Pts',(2.75619335349672,-2.57658041242155,5.40100865009198));
#16870=CARTESIAN_POINT('Ctrl Pts',(2.76803982089465,-2.58829135908692,5.40409416353221));
#16871=CARTESIAN_POINT('Ctrl Pts',(2.78,-2.6,5.40717967697245));
#16872=CARTESIAN_POINT('Ctrl Pts',(2.78,-2.6,5.40717967697245));
#16873=CARTESIAN_POINT('Ctrl Pts',(2.76803982089465,-2.58829135908692,5.40409416353221));
#16874=CARTESIAN_POINT('Ctrl Pts',(2.75619335349672,-2.57658041242155,5.40100865009198));
#16875=CARTESIAN_POINT('Ctrl Pts',(2.74442178368681,-2.56486895213672,5.39792313665174));
#16876=CARTESIAN_POINT('Origin',(1.4375,2.58232233047034,0.0873223304703362));
#16877=CARTESIAN_POINT('',(2.83,2.6,0.13));
#16878=CARTESIAN_POINT('',(3.21192363215214,2.75819794822821,0.511923632152139));
#16879=CARTESIAN_POINT('',(5.62,2.6,0.13));
#16880=CARTESIAN_POINT('',(1.4375,2.6,0.13));
#16881=CARTESIAN_POINT('',(3.45077738091134,3.49852142863302,2.29922261908869));
#16882=CARTESIAN_POINT('Origin',(2.78732233047034,2.58232233047034,3.28125));
#16883=CARTESIAN_POINT('',(2.74464466094067,2.56464466094067,5.36678788880707));
#16884=CARTESIAN_POINT('',(2.74464466094067,2.56464466094067,3.28125));
#16885=CARTESIAN_POINT('',(2.83,2.6,5.36678788880707));
#16886=CARTESIAN_POINT('',(2.83,2.6,5.36678788880707));
#16887=CARTESIAN_POINT('',(2.83,2.6,3.28125));
#16888=CARTESIAN_POINT('Ctrl Pts',(2.74442178368363,2.56486895213994,5.39792313687514));
#16889=CARTESIAN_POINT('Ctrl Pts',(2.74456950540177,2.56471935013366,5.38754472085245));
#16890=CARTESIAN_POINT('Ctrl Pts',(2.74464466094067,2.56464466094067,5.37716630482976));
#16891=CARTESIAN_POINT('Ctrl Pts',(2.74464466094067,2.56464466094067,5.36678788880707));
#16892=CARTESIAN_POINT('Ctrl Pts',(2.77294785578909,2.57657930142663,5.39792313687514));
#16893=CARTESIAN_POINT('Ctrl Pts',(2.77304633693452,2.57647956675577,5.38754472085245));
#16894=CARTESIAN_POINT('Ctrl Pts',(2.77309644062712,2.57642977396045,5.37716630482976));
#16895=CARTESIAN_POINT('Ctrl Pts',(2.77309644062712,2.57642977396045,5.36678788880707));
#16896=CARTESIAN_POINT('Ctrl Pts',(2.80147392789454,2.58828965071331,5.39792313687514));
#16897=CARTESIAN_POINT('Ctrl Pts',(2.80152316846726,2.58823978337789,5.38754472085245));
#16898=CARTESIAN_POINT('Ctrl Pts',(2.80154822031356,2.58821488698022,5.37716630482976));
#16899=CARTESIAN_POINT('Ctrl Pts',(2.80154822031356,2.58821488698022,5.36678788880707));
#16900=CARTESIAN_POINT('Ctrl Pts',(2.83,2.6,5.39792313687514));
#16901=CARTESIAN_POINT('Ctrl Pts',(2.83,2.6,5.38754472085245));
#16902=CARTESIAN_POINT('Ctrl Pts',(2.83,2.6,5.37716630482976));
#16903=CARTESIAN_POINT('Ctrl Pts',(2.83,2.6,5.36678788880707));
#16904=CARTESIAN_POINT('',(2.74442178368363,2.56486895213994,5.39792313687514));
#16905=CARTESIAN_POINT('',(2.83,2.6,5.39792313687514));
#16906=CARTESIAN_POINT('Ctrl Pts',(2.74442178368363,2.56486895213994,5.39792313687514));
#16907=CARTESIAN_POINT('Ctrl Pts',(2.77294785578909,2.57657930142663,5.39792313687514));
#16908=CARTESIAN_POINT('Ctrl Pts',(2.80147392789454,2.58828965071331,5.39792313687514));
#16909=CARTESIAN_POINT('Ctrl Pts',(2.83,2.6,5.39792313687514));
#16910=CARTESIAN_POINT('Ctrl Pts',(2.83,2.6,5.39792313687514));
#16911=CARTESIAN_POINT('Ctrl Pts',(2.83,2.6,5.38754472085245));
#16912=CARTESIAN_POINT('Ctrl Pts',(2.83,2.6,5.37716630482976));
#16913=CARTESIAN_POINT('Ctrl Pts',(2.83,2.6,5.36678788880707));
#16914=CARTESIAN_POINT('Ctrl Pts',(2.74464466094067,2.56464466094067,5.36678788880707));
#16915=CARTESIAN_POINT('Ctrl Pts',(2.74464466094067,2.56464466094067,5.37716630482976));
#16916=CARTESIAN_POINT('Ctrl Pts',(2.74456950540177,2.56471935013366,5.38754472085245));
#16917=CARTESIAN_POINT('Ctrl Pts',(2.74442178368363,2.56486895213994,5.39792313687514));
#16918=CARTESIAN_POINT('Ctrl Pts',(2.74442178368363,2.56486895213994,5.39792313687514));
#16919=CARTESIAN_POINT('Ctrl Pts',(2.75619335349611,2.57658041242369,5.40100865024091));
#16920=CARTESIAN_POINT('Ctrl Pts',(2.76803982089572,2.58829135908796,5.40409416360668));
#16921=CARTESIAN_POINT('Ctrl Pts',(2.78,2.6,5.40717967697245));
#16922=CARTESIAN_POINT('Ctrl Pts',(2.77294785578909,2.57657930142663,5.39792313687514));
#16923=CARTESIAN_POINT('Ctrl Pts',(2.77524001344185,2.58438694161579,5.40100865024091));
#16924=CARTESIAN_POINT('Ctrl Pts',(2.77758210281937,2.59219423939197,5.40409416360668));
#16925=CARTESIAN_POINT('Ctrl Pts',(2.78,2.6,5.40717967697245));
#16926=CARTESIAN_POINT('Ctrl Pts',(2.80147392789454,2.58828965071331,5.39792313687514));
#16927=CARTESIAN_POINT('Ctrl Pts',(2.79428667338759,2.5921934708079,5.40100865024091));
#16928=CARTESIAN_POINT('Ctrl Pts',(2.78712438474302,2.59609711969599,5.40409416360668));
#16929=CARTESIAN_POINT('Ctrl Pts',(2.78,2.6,5.40717967697245));
#16930=CARTESIAN_POINT('Ctrl Pts',(2.83,2.6,5.39792313687514));
#16931=CARTESIAN_POINT('Ctrl Pts',(2.81333333333333,2.6,5.40100865024091));
#16932=CARTESIAN_POINT('Ctrl Pts',(2.79666666666667,2.6,5.40409416360668));
#16933=CARTESIAN_POINT('Ctrl Pts',(2.78,2.6,5.40717967697245));
#16934=CARTESIAN_POINT('',(2.78,2.6,5.40717967697245));
#16935=CARTESIAN_POINT('Ctrl Pts',(2.74442178368363,2.56486895213994,5.39792313687514));
#16936=CARTESIAN_POINT('Ctrl Pts',(2.75619335349611,2.57658041242369,5.40100865024091));
#16937=CARTESIAN_POINT('Ctrl Pts',(2.76803982089572,2.58829135908796,5.40409416360668));
#16938=CARTESIAN_POINT('Ctrl Pts',(2.78,2.6,5.40717967697245));
#16939=CARTESIAN_POINT('Ctrl Pts',(2.78,2.6,5.40717967697245));
#16940=CARTESIAN_POINT('Ctrl Pts',(2.79666666666667,2.6,5.40409416360668));
#16941=CARTESIAN_POINT('Ctrl Pts',(2.81333333333333,2.6,5.40100865024091));
#16942=CARTESIAN_POINT('Ctrl Pts',(2.83,2.6,5.39792313687514));
#16943=CARTESIAN_POINT('Origin',(0.,2.6,4.375));
#16944=CARTESIAN_POINT('',(2.42414283215735,2.6,6.0885134021324));
#16945=CARTESIAN_POINT('Ctrl Pts',(2.42414283215735,2.6,6.0885134021324));
#16946=CARTESIAN_POINT('Ctrl Pts',(2.47340183676993,2.6,6.03819996865039));
#16947=CARTESIAN_POINT('Ctrl Pts',(2.57677270784915,2.6,5.92754153415384));
#16948=CARTESIAN_POINT('Ctrl Pts',(2.66963073857957,2.6,5.79083331222164));
#16949=CARTESIAN_POINT('Ctrl Pts',(2.7334746318431,2.6,5.65860602138498));
#16950=CARTESIAN_POINT('Ctrl Pts',(2.77172491031876,2.6,5.54191130109615));
#16951=CARTESIAN_POINT('Ctrl Pts',(2.78,2.6,5.44464477671191));
#16952=CARTESIAN_POINT('Ctrl Pts',(2.78,2.6,5.40717967697245));
#16953=CARTESIAN_POINT('',(2.3,2.6,6.1));
#16954=CARTESIAN_POINT('Ctrl Pts',(2.3,2.6,6.1));
#16955=CARTESIAN_POINT('Ctrl Pts',(2.34138094405245,2.6,6.09617113404413));
#16956=CARTESIAN_POINT('Ctrl Pts',(2.3827618881049,2.6,6.09234226808826));
#16957=CARTESIAN_POINT('Ctrl Pts',(2.42414283215735,2.6,6.0885134021324));
#16958=CARTESIAN_POINT('',(-2.3,2.6,6.1));
#16959=CARTESIAN_POINT('',(1.35,2.6,6.1));
#16960=CARTESIAN_POINT('',(-2.42414283238944,2.6,6.08851340189533));
#16961=CARTESIAN_POINT('Ctrl Pts',(-2.42414283238944,2.6,6.08851340189533));
#16962=CARTESIAN_POINT('Ctrl Pts',(-2.38276188825963,2.6,6.09234226793022));
#16963=CARTESIAN_POINT('Ctrl Pts',(-2.34138094412981,2.6,6.09617113396511));
#16964=CARTESIAN_POINT('Ctrl Pts',(-2.3,2.6,6.1));
#16965=CARTESIAN_POINT('',(-2.78,2.6,5.40717967697245));
#16966=CARTESIAN_POINT('Ctrl Pts',(-2.78,2.6,5.40717967697245));
#16967=CARTESIAN_POINT('Ctrl Pts',(-2.78,2.6,5.44865469871872));
#16968=CARTESIAN_POINT('Ctrl Pts',(-2.77175013108469,2.6,5.53495446115542));
#16969=CARTESIAN_POINT('Ctrl Pts',(-2.7315293753489,2.6,5.66466680090526));
#16970=CARTESIAN_POINT('Ctrl Pts',(-2.66093134122624,2.6,5.80894311125375));
#16971=CARTESIAN_POINT('Ctrl Pts',(-2.5873706385557,2.6,5.90812597923557));
#16972=CARTESIAN_POINT('Ctrl Pts',(-2.4973849688124,2.6,6.01246084453175));
#16973=CARTESIAN_POINT('Ctrl Pts',(-2.46022125233163,2.6,6.05166269416306));
#16974=CARTESIAN_POINT('Ctrl Pts',(-2.42414283238944,2.6,6.08851340189533));
#16975=CARTESIAN_POINT('',(-2.83,2.6,5.39792313665175));
#16976=CARTESIAN_POINT('Ctrl Pts',(-2.83,2.6,5.39792313665175));
#16977=CARTESIAN_POINT('Ctrl Pts',(-2.81333333333333,2.6,5.40100865009198));
#16978=CARTESIAN_POINT('Ctrl Pts',(-2.79666666666667,2.6,5.40409416353221));
#16979=CARTESIAN_POINT('Ctrl Pts',(-2.78,2.6,5.40717967697245));
#16980=CARTESIAN_POINT('',(-2.83,2.6,5.36678788880707));
#16981=CARTESIAN_POINT('Ctrl Pts',(-2.83,2.6,5.36678788880707));
#16982=CARTESIAN_POINT('Ctrl Pts',(-2.83,2.6,5.37716630475529));
#16983=CARTESIAN_POINT('Ctrl Pts',(-2.83,2.6,5.38754472070352));
#16984=CARTESIAN_POINT('Ctrl Pts',(-2.83,2.6,5.39792313665175));
#16985=CARTESIAN_POINT('',(-2.83,2.6,0.13));
#16986=CARTESIAN_POINT('',(-2.83,2.6,4.70625));
#16987=CARTESIAN_POINT('',(-5.62,2.6,0.13));
#16988=CARTESIAN_POINT('',(-0.675,2.6,0.13));
#16989=CARTESIAN_POINT('',(-5.62,2.6,8.62));
#16990=CARTESIAN_POINT('',(-5.62,2.6,3.28125));
#16991=CARTESIAN_POINT('',(5.62,2.6,8.62));
#16992=CARTESIAN_POINT('',(-1.4375,2.6,8.62));
#16993=CARTESIAN_POINT('',(5.62,2.6,5.46875));
#16994=CARTESIAN_POINT('',(4.21,2.6,1.));
#16995=CARTESIAN_POINT('Origin',(4.6,2.6,1.));
#16996=CARTESIAN_POINT('',(-4.99,2.6,1.));
#16997=CARTESIAN_POINT('Origin',(-4.6,2.6,1.));
#16998=CARTESIAN_POINT('',(4.21,2.6,7.75));
#16999=CARTESIAN_POINT('Origin',(4.6,2.6,7.75));
#17000=CARTESIAN_POINT('',(-4.99,2.6,7.75));
#17001=CARTESIAN_POINT('Origin',(-4.6,2.6,7.75));
#17002=CARTESIAN_POINT('Ctrl Pts',(2.69829980684391,2.52001806864527,5.40717967697245));
#17003=CARTESIAN_POINT('Ctrl Pts',(2.69942945076934,2.51999405556084,5.39371574758399));
#17004=CARTESIAN_POINT('Ctrl Pts',(2.7,2.52,5.38025181819553));
#17005=CARTESIAN_POINT('Ctrl Pts',(2.7,2.52,5.36678788880707));
#17006=CARTESIAN_POINT('Ctrl Pts',(2.7255332045626,2.54667871243018,5.40717967697245));
#17007=CARTESIAN_POINT('Ctrl Pts',(2.72628630051289,2.54666270370723,5.39371574758399));
#17008=CARTESIAN_POINT('Ctrl Pts',(2.72666666666667,2.54666666666667,5.38025181819553));
#17009=CARTESIAN_POINT('Ctrl Pts',(2.72666666666667,2.54666666666667,5.36678788880707));
#17010=CARTESIAN_POINT('Ctrl Pts',(2.7527666022813,2.57333935621509,5.40717967697245));
#17011=CARTESIAN_POINT('Ctrl Pts',(2.75314315025645,2.57333135185361,5.39371574758399));
#17012=CARTESIAN_POINT('Ctrl Pts',(2.75333333333333,2.57333333333333,5.38025181819553));
#17013=CARTESIAN_POINT('Ctrl Pts',(2.75333333333333,2.57333333333333,5.36678788880707));
#17014=CARTESIAN_POINT('Ctrl Pts',(2.78,2.6,5.40717967697245));
#17015=CARTESIAN_POINT('Ctrl Pts',(2.78,2.6,5.39371574758399));
#17016=CARTESIAN_POINT('Ctrl Pts',(2.78,2.6,5.38025181819553));
#17017=CARTESIAN_POINT('Ctrl Pts',(2.78,2.6,5.36678788880707));
#17018=CARTESIAN_POINT('',(2.7,2.52,5.36678788880707));
#17019=CARTESIAN_POINT('',(2.69829980684391,2.52001806864527,5.40717967697245));
#17020=CARTESIAN_POINT('Ctrl Pts',(2.7,2.52,5.36678788880707));
#17021=CARTESIAN_POINT('Ctrl Pts',(2.7,2.52,5.38025181819553));
#17022=CARTESIAN_POINT('Ctrl Pts',(2.69942945076934,2.51999405556084,5.39371574758399));
#17023=CARTESIAN_POINT('Ctrl Pts',(2.69829980684391,2.52001806864527,5.40717967697245));
#17024=CARTESIAN_POINT('',(2.78,2.6,5.40717967697245));
#17025=CARTESIAN_POINT('Origin',(-1.4375,2.58232233047034,8.66267766952966));
#17026=CARTESIAN_POINT('',(5.68306019374819,2.57387961250363,8.68306019374819));
#17027=CARTESIAN_POINT('',(4.88692077572932,2.01092403125258,10.0421551930181));
#17028=CARTESIAN_POINT('',(3.29248197949184,3.56408953076227,6.29248197949182));
#17029=CARTESIAN_POINT('',(-3.45077738091134,3.49852142863302,6.45077738091131));
#17030=CARTESIAN_POINT('Origin',(5.66267766952966,2.58232233047034,5.46875));
#17031=CARTESIAN_POINT('',(6.3287007863016,2.3064465226494,8.30485269104902));
#17032=CARTESIAN_POINT('Origin',(5.75,2.52,8.67));
#17033=CARTESIAN_POINT('Origin',(-0.675,2.58232233047034,0.0873223304703362));
#17034=CARTESIAN_POINT('',(-3.77888057658085,3.36261663512876,1.97111942341917));
#17035=CARTESIAN_POINT('',(-3.36446283715638,2.82138175573458,0.664462837156383));
#17036=CARTESIAN_POINT('Origin',(-5.66267766952966,2.58232233047034,3.28125));
#17037=CARTESIAN_POINT('',(-5.70535533905933,2.56464466094067,3.28125));
#17038=CARTESIAN_POINT('Origin',(-2.78732233047034,2.58232233047034,4.70625));
#17039=CARTESIAN_POINT('',(-2.83,2.6,5.36678788880707));
#17040=CARTESIAN_POINT('Ctrl Pts',(-2.74464466094067,2.56464466094067,5.36678788880707));
#17041=CARTESIAN_POINT('Ctrl Pts',(-2.74464466094067,2.56464466094067,5.37716630475529));
#17042=CARTESIAN_POINT('Ctrl Pts',(-2.74456950540286,2.56471935013259,5.38754472070352));
#17043=CARTESIAN_POINT('Ctrl Pts',(-2.74442178368681,2.56486895213672,5.39792313665175));
#17044=CARTESIAN_POINT('Ctrl Pts',(-2.77309644062712,2.57642977396045,5.36678788880707));
#17045=CARTESIAN_POINT('Ctrl Pts',(-2.77309644062712,2.57642977396045,5.37716630475529));
#17046=CARTESIAN_POINT('Ctrl Pts',(-2.77304633693524,2.57647956675506,5.38754472070352));
#17047=CARTESIAN_POINT('Ctrl Pts',(-2.77294785579121,2.57657930142448,5.39792313665175));
#17048=CARTESIAN_POINT('Ctrl Pts',(-2.80154822031356,2.58821488698022,5.36678788880707));
#17049=CARTESIAN_POINT('Ctrl Pts',(-2.80154822031356,2.58821488698022,5.37716630475529));
#17050=CARTESIAN_POINT('Ctrl Pts',(-2.80152316846762,2.58823978337753,5.38754472070352));
#17051=CARTESIAN_POINT('Ctrl Pts',(-2.8014739278956,2.58828965071224,5.39792313665175));
#17052=CARTESIAN_POINT('Ctrl Pts',(-2.83,2.6,5.36678788880707));
#17053=CARTESIAN_POINT('Ctrl Pts',(-2.83,2.6,5.37716630475529));
#17054=CARTESIAN_POINT('Ctrl Pts',(-2.83,2.6,5.38754472070352));
#17055=CARTESIAN_POINT('Ctrl Pts',(-2.83,2.6,5.39792313665175));
#17056=CARTESIAN_POINT('',(-2.74442178368681,2.56486895213672,5.39792313665175));
#17057=CARTESIAN_POINT('Ctrl Pts',(-2.83,2.6,5.39792313665175));
#17058=CARTESIAN_POINT('Ctrl Pts',(-2.8014739278956,2.58828965071224,5.39792313665175));
#17059=CARTESIAN_POINT('Ctrl Pts',(-2.77294785579121,2.57657930142448,5.39792313665175));
#17060=CARTESIAN_POINT('Ctrl Pts',(-2.74442178368681,2.56486895213672,5.39792313665175));
#17061=CARTESIAN_POINT('Ctrl Pts',(-2.74442178368681,2.56486895213672,5.39792313665175));
#17062=CARTESIAN_POINT('Ctrl Pts',(-2.74456950540286,2.56471935013259,5.38754472070352));
#17063=CARTESIAN_POINT('Ctrl Pts',(-2.74464466094067,2.56464466094067,5.37716630475529));
#17064=CARTESIAN_POINT('Ctrl Pts',(-2.74464466094067,2.56464466094067,5.36678788880707));
#17065=CARTESIAN_POINT('Ctrl Pts',(-2.83,2.6,5.39792313665175));
#17066=CARTESIAN_POINT('Ctrl Pts',(-2.81333333333333,2.6,5.40100865009198));
#17067=CARTESIAN_POINT('Ctrl Pts',(-2.79666666666667,2.6,5.40409416353221));
#17068=CARTESIAN_POINT('Ctrl Pts',(-2.78,2.6,5.40717967697245));
#17069=CARTESIAN_POINT('Ctrl Pts',(-2.8014739278956,2.58828965071224,5.39792313665175));
#17070=CARTESIAN_POINT('Ctrl Pts',(-2.7942866733878,2.59219347080718,5.40100865009198));
#17071=CARTESIAN_POINT('Ctrl Pts',(-2.78712438474266,2.59609711969564,5.40409416353221));
#17072=CARTESIAN_POINT('Ctrl Pts',(-2.78,2.6,5.40717967697245));
#17073=CARTESIAN_POINT('Ctrl Pts',(-2.77294785579121,2.57657930142448,5.39792313665175));
#17074=CARTESIAN_POINT('Ctrl Pts',(-2.77524001344226,2.58438694161436,5.40100865009198));
#17075=CARTESIAN_POINT('Ctrl Pts',(-2.77758210281866,2.59219423939128,5.40409416353221));
#17076=CARTESIAN_POINT('Ctrl Pts',(-2.78,2.6,5.40717967697245));
#17077=CARTESIAN_POINT('Ctrl Pts',(-2.74442178368681,2.56486895213672,5.39792313665175));
#17078=CARTESIAN_POINT('Ctrl Pts',(-2.75619335349672,2.57658041242155,5.40100865009198));
#17079=CARTESIAN_POINT('Ctrl Pts',(-2.76803982089465,2.58829135908692,5.40409416353221));
#17080=CARTESIAN_POINT('Ctrl Pts',(-2.78,2.6,5.40717967697245));
#17081=CARTESIAN_POINT('Ctrl Pts',(-2.78,2.6,5.40717967697245));
#17082=CARTESIAN_POINT('Ctrl Pts',(-2.76803982089465,2.58829135908692,5.40409416353221));
#17083=CARTESIAN_POINT('Ctrl Pts',(-2.75619335349672,2.57658041242155,5.40100865009198));
#17084=CARTESIAN_POINT('Ctrl Pts',(-2.74442178368681,2.56486895213672,5.39792313665175));
#17085=CARTESIAN_POINT('Origin',(-4.6,2.57,7.75));
#17086=CARTESIAN_POINT('',(-4.93,2.54,7.75));
#17087=CARTESIAN_POINT('',(-4.96,2.57,7.75));
#17088=CARTESIAN_POINT('Origin',(-4.6,2.54,7.75));
#17089=CARTESIAN_POINT('Origin',(-4.6,0.,7.75));
#17090=CARTESIAN_POINT('',(-4.93,-2.54,7.75));
#17091=CARTESIAN_POINT('Origin',(-4.6,-2.54,7.75));
#17092=CARTESIAN_POINT('',(-4.93,0.,7.75));
#17093=CARTESIAN_POINT('Origin',(-4.6,-2.57,7.75));
#17094=CARTESIAN_POINT('',(-4.96,-2.57,7.75));
#17095=CARTESIAN_POINT('Origin',(4.6,2.57,1.));
#17096=CARTESIAN_POINT('',(4.27,2.54,1.));
#17097=CARTESIAN_POINT('',(4.24,2.57,1.));
#17098=CARTESIAN_POINT('Origin',(4.6,2.54,1.));
#17099=CARTESIAN_POINT('Origin',(4.6,0.,1.));
#17100=CARTESIAN_POINT('',(4.27,-2.54,1.));
#17101=CARTESIAN_POINT('Origin',(4.6,-2.54,1.));
#17102=CARTESIAN_POINT('',(4.27,0.,1.));
#17103=CARTESIAN_POINT('Origin',(4.6,-2.57,1.));
#17104=CARTESIAN_POINT('',(4.24,-2.57,1.));
#17105=CARTESIAN_POINT('Origin',(4.6,2.57,7.75));
#17106=CARTESIAN_POINT('',(4.27,2.54,7.75));
#17107=CARTESIAN_POINT('',(4.24,2.57,7.75));
#17108=CARTESIAN_POINT('Origin',(4.6,2.54,7.75));
#17109=CARTESIAN_POINT('Origin',(4.6,0.,7.75));
#17110=CARTESIAN_POINT('',(4.27,-2.54,7.75));
#17111=CARTESIAN_POINT('Origin',(4.6,-2.54,7.75));
#17112=CARTESIAN_POINT('',(4.27,0.,7.75));
#17113=CARTESIAN_POINT('Origin',(4.6,-2.57,7.75));
#17114=CARTESIAN_POINT('',(4.24,-2.57,7.75));
#17115=CARTESIAN_POINT('Origin',(-4.6,2.57,1.));
#17116=CARTESIAN_POINT('',(-4.93,2.54,1.));
#17117=CARTESIAN_POINT('',(-4.96,2.57,1.));
#17118=CARTESIAN_POINT('Origin',(-4.6,2.54,1.));
#17119=CARTESIAN_POINT('Origin',(-4.6,0.,1.));
#17120=CARTESIAN_POINT('',(-4.93,-2.54,1.));
#17121=CARTESIAN_POINT('Origin',(-4.6,-2.54,1.));
#17122=CARTESIAN_POINT('',(-4.93,0.,1.));
#17123=CARTESIAN_POINT('Origin',(-4.6,-2.57,1.));
#17124=CARTESIAN_POINT('',(-4.96,-2.57,1.));
#17125=CARTESIAN_POINT('Origin',(0.,0.,5.7));
#17126=CARTESIAN_POINT('',(-1.35,-1.65327317884893E-16,5.7));
#17127=CARTESIAN_POINT('Origin',(0.,0.,5.7));
#17128=CARTESIAN_POINT('',(-1.3,-1.59204083889156E-16,5.75));
#17129=CARTESIAN_POINT('',(-1.35,-1.65327317884893E-16,5.7));
#17130=CARTESIAN_POINT('Origin',(0.,0.,5.75));
#17131=CARTESIAN_POINT('Origin',(0.,0.,6.125));
#17132=CARTESIAN_POINT('',(-1.3,-1.59204083889156E-16,6.5));
#17133=CARTESIAN_POINT('',(-1.3,-1.59204083889156E-16,6.125));
#17134=CARTESIAN_POINT('Origin',(0.,0.,6.5));
#17135=CARTESIAN_POINT('Origin',(0.7,0.,6.5));
#17136=CARTESIAN_POINT('',(-0.7,-8.57252759403147E-17,6.5));
#17137=CARTESIAN_POINT('Origin',(0.,0.,6.5));
#17138=CARTESIAN_POINT('Origin',(0.,0.,7.225));
#17139=CARTESIAN_POINT('',(-0.7,-8.57252759403147E-17,7.95));
#17140=CARTESIAN_POINT('',(-0.7,-8.57252759403147E-17,7.225));
#17141=CARTESIAN_POINT('Origin',(0.,0.,7.95));
#17142=CARTESIAN_POINT('Origin',(1.3,0.,7.95));
#17143=CARTESIAN_POINT('',(-1.3,-1.59204083889156E-16,7.95));
#17144=CARTESIAN_POINT('Origin',(0.,0.,7.95));
#17145=CARTESIAN_POINT('Origin',(0.,0.,8.325));
#17146=CARTESIAN_POINT('',(-1.3,-1.59204083889156E-16,8.7));
#17147=CARTESIAN_POINT('',(-1.3,-1.59204083889156E-16,8.325));
#17148=CARTESIAN_POINT('Origin',(0.,0.,8.7));
#17149=CARTESIAN_POINT('Origin',(0.,0.,8.75));
#17150=CARTESIAN_POINT('',(-1.35,1.65327317884893E-16,8.75));
#17151=CARTESIAN_POINT('',(-1.35,-1.65327317884893E-16,8.75));
#17152=CARTESIAN_POINT('Origin',(0.,0.,8.75));
#17153=CARTESIAN_POINT('Origin',(-2.7,0.,3.));
#17154=CARTESIAN_POINT('',(-2.75,-1.59204083889156E-16,1.7));
#17155=CARTESIAN_POINT('',(-2.7,-1.65327317884893E-16,1.65));
#17156=CARTESIAN_POINT('Origin',(-2.75,0.,3.));
#17157=CARTESIAN_POINT('Origin',(-3.125,0.,3.));
#17158=CARTESIAN_POINT('',(-3.5,-1.59204083889156E-16,1.7));
#17159=CARTESIAN_POINT('',(-3.125,-1.59204083889156E-16,1.7));
#17160=CARTESIAN_POINT('Origin',(-3.5,0.,3.));
#17161=CARTESIAN_POINT('Origin',(-3.5,0.,3.7));
#17162=CARTESIAN_POINT('',(-3.5,-8.57252759403147E-17,2.3));
#17163=CARTESIAN_POINT('Origin',(-3.5,0.,3.));
#17164=CARTESIAN_POINT('Origin',(-4.225,0.,3.));
#17165=CARTESIAN_POINT('',(-4.95,-8.57252759403147E-17,2.3));
#17166=CARTESIAN_POINT('',(-4.225,-8.57252759403147E-17,2.3));
#17167=CARTESIAN_POINT('Origin',(-4.95,0.,3.));
#17168=CARTESIAN_POINT('Origin',(-4.95,0.,4.3));
#17169=CARTESIAN_POINT('',(-4.95,-1.59204083889156E-16,1.7));
#17170=CARTESIAN_POINT('Origin',(-4.95,0.,3.));
#17171=CARTESIAN_POINT('Origin',(-5.325,0.,3.));
#17172=CARTESIAN_POINT('',(-5.7,-1.59204083889156E-16,1.7));
#17173=CARTESIAN_POINT('',(-5.325,-1.59204083889156E-16,1.7));
#17174=CARTESIAN_POINT('Origin',(-5.7,0.,3.));
#17175=CARTESIAN_POINT('Origin',(-5.75,0.,3.));
#17176=CARTESIAN_POINT('',(-5.75,-1.65327317884893E-16,1.65));
#17177=CARTESIAN_POINT('Origin',(5.75,0.,3.));
#17178=CARTESIAN_POINT('',(5.7,-1.59204083889156E-16,1.7));
#17179=CARTESIAN_POINT('',(5.75,-1.65327317884893E-16,1.65));
#17180=CARTESIAN_POINT('Origin',(5.7,0.,3.));
#17181=CARTESIAN_POINT('Origin',(5.325,0.,3.));
#17182=CARTESIAN_POINT('',(4.95,-1.59204083889156E-16,1.7));
#17183=CARTESIAN_POINT('',(5.325,-1.59204083889156E-16,1.7));
#17184=CARTESIAN_POINT('Origin',(4.95,0.,3.));
#17185=CARTESIAN_POINT('Origin',(4.95,0.,3.7));
#17186=CARTESIAN_POINT('',(4.95,-8.57252759403147E-17,2.3));
#17187=CARTESIAN_POINT('Origin',(4.95,0.,3.));
#17188=CARTESIAN_POINT('Origin',(4.225,0.,3.));
#17189=CARTESIAN_POINT('',(3.5,-8.57252759403147E-17,2.3));
#17190=CARTESIAN_POINT('',(4.225,-8.57252759403147E-17,2.3));
#17191=CARTESIAN_POINT('Origin',(3.5,0.,3.));
#17192=CARTESIAN_POINT('Origin',(3.5,0.,4.3));
#17193=CARTESIAN_POINT('',(3.5,-1.59204083889156E-16,1.7));
#17194=CARTESIAN_POINT('Origin',(3.5,0.,3.));
#17195=CARTESIAN_POINT('Origin',(3.125,0.,3.));
#17196=CARTESIAN_POINT('',(2.75,-1.59204083889156E-16,1.7));
#17197=CARTESIAN_POINT('',(3.125,-1.59204083889156E-16,1.7));
#17198=CARTESIAN_POINT('Origin',(2.75,0.,3.));
#17199=CARTESIAN_POINT('Origin',(2.7,0.,3.));
#17200=CARTESIAN_POINT('',(2.7,-1.65327317884893E-16,1.65));
#17201=CARTESIAN_POINT('Ctrl Pts',(-2.31142159057266,-2.58116161377225,
5.9781544825592));
#17202=CARTESIAN_POINT('Ctrl Pts',(-2.36128434130633,-2.56784999958484,
5.93183474087413));
#17203=CARTESIAN_POINT('Ctrl Pts',(-2.43995511674461,-2.5495376072066,5.86291013494394));
#17204=CARTESIAN_POINT('Ctrl Pts',(-2.53391137386914,-2.53448278521197,
5.76471507012624));
#17205=CARTESIAN_POINT('Ctrl Pts',(-2.59241291603181,-2.52736920010306,
5.69068137785945));
#17206=CARTESIAN_POINT('Ctrl Pts',(-2.64432087785964,-2.52278488329719,
5.60511511887677));
#17207=CARTESIAN_POINT('Ctrl Pts',(-2.68329779044149,-2.52048776381013,
5.50684199397487));
#17208=CARTESIAN_POINT('Ctrl Pts',(-2.69557514809684,-2.5200759873036,5.43965416929022));
#17209=CARTESIAN_POINT('Ctrl Pts',(-2.69829980684391,-2.52001806864527,
5.40717967697245));
#17210=CARTESIAN_POINT('Ctrl Pts',(-2.34899533776733,-2.58744107584817,
6.01494078908382));
#17211=CARTESIAN_POINT('Ctrl Pts',(-2.39865683979399,-2.5785666663899,5.96728981679977));
#17212=CARTESIAN_POINT('Ctrl Pts',(-2.4766857923441,-2.5663584048044,5.89405976020693));
#17213=CARTESIAN_POINT('Ctrl Pts',(-2.56915127374486,-2.55632185680798,
5.78808953647345));
#17214=CARTESIAN_POINT('Ctrl Pts',(-2.62632274601193,-2.55157946673537,
5.70829633719456));
#17215=CARTESIAN_POINT('Ctrl Pts',(-2.67648636529298,-2.54852325553146,
5.61659793937325));
#17216=CARTESIAN_POINT('Ctrl Pts',(-2.71319808109984,-2.54699184254009,
5.51215507085786));
#17217=CARTESIAN_POINT('Ctrl Pts',(-2.72371676539789,-2.54671732486907,
5.44131770509747));
#17218=CARTESIAN_POINT('Ctrl Pts',(-2.7255332045626,-2.54667871243018,5.40717967697245));
#17219=CARTESIAN_POINT('Ctrl Pts',(-2.38656908496201,-2.59372053792408,
6.05172709560844));
#17220=CARTESIAN_POINT('Ctrl Pts',(-2.43602933828165,-2.58928333319495,
6.0027448927254));
#17221=CARTESIAN_POINT('Ctrl Pts',(-2.5134164679436,-2.5831792024022,5.92520938546991));
#17222=CARTESIAN_POINT('Ctrl Pts',(-2.60439117362058,-2.57816092840399,
5.81146400282065));
#17223=CARTESIAN_POINT('Ctrl Pts',(-2.66023257599205,-2.57578973336769,
5.72591129652966));
#17224=CARTESIAN_POINT('Ctrl Pts',(-2.70865185272632,-2.57426162776573,
5.62808075986973));
#17225=CARTESIAN_POINT('Ctrl Pts',(-2.7430983717582,-2.57349592127004,5.51746814774084));
#17226=CARTESIAN_POINT('Ctrl Pts',(-2.75185838269895,-2.57335866243453,
5.44298124090471));
#17227=CARTESIAN_POINT('Ctrl Pts',(-2.7527666022813,-2.57333935621509,5.40717967697245));
#17228=CARTESIAN_POINT('Ctrl Pts',(-2.42414283215669,-2.6,6.08851340213307));
#17229=CARTESIAN_POINT('Ctrl Pts',(-2.47340183676932,-2.6,6.03819996865104));
#17230=CARTESIAN_POINT('Ctrl Pts',(-2.55014714354309,-2.6,5.9563590107329));
#17231=CARTESIAN_POINT('Ctrl Pts',(-2.6396310734963,-2.6,5.83483846916786));
#17232=CARTESIAN_POINT('Ctrl Pts',(-2.69414240597218,-2.6,5.74352625586477));
#17233=CARTESIAN_POINT('Ctrl Pts',(-2.74081734015966,-2.6,5.6395635803662));
#17234=CARTESIAN_POINT('Ctrl Pts',(-2.77299866241655,-2.6,5.52278122462383));
#17235=CARTESIAN_POINT('Ctrl Pts',(-2.78,-2.6,5.44464477671195));
#17236=CARTESIAN_POINT('Ctrl Pts',(-2.78,-2.6,5.40717967697245));
#17237=CARTESIAN_POINT('',(-2.31142159057266,-2.58116161377225,5.9781544825592));
#17238=CARTESIAN_POINT('Ctrl Pts',(-2.31142159057266,-2.58116161377225,
5.9781544825592));
#17239=CARTESIAN_POINT('Ctrl Pts',(-2.34899533776733,-2.58744107584817,
6.01494078908382));
#17240=CARTESIAN_POINT('Ctrl Pts',(-2.38656908496201,-2.59372053792408,
6.05172709560844));
#17241=CARTESIAN_POINT('Ctrl Pts',(-2.42414283215669,-2.6,6.08851340213307));
#17242=CARTESIAN_POINT('Ctrl Pts',(-2.69829980684391,-2.52001806864527,
5.40717967697245));
#17243=CARTESIAN_POINT('Ctrl Pts',(-2.69557514809684,-2.5200759873036,5.43965416929022));
#17244=CARTESIAN_POINT('Ctrl Pts',(-2.68329779044149,-2.52048776381013,
5.50684199397487));
#17245=CARTESIAN_POINT('Ctrl Pts',(-2.64432087785964,-2.52278488329719,
5.60511511887677));
#17246=CARTESIAN_POINT('Ctrl Pts',(-2.59241291603181,-2.52736920010306,
5.69068137785945));
#17247=CARTESIAN_POINT('Ctrl Pts',(-2.53391137386914,-2.53448278521197,
5.76471507012624));
#17248=CARTESIAN_POINT('Ctrl Pts',(-2.43995511674461,-2.5495376072066,5.86291013494394));
#17249=CARTESIAN_POINT('Ctrl Pts',(-2.36128434130633,-2.56784999958484,
5.93183474087413));
#17250=CARTESIAN_POINT('Ctrl Pts',(-2.31142159057266,-2.58116161377225,
5.9781544825592));
#17251=CARTESIAN_POINT('Ctrl Pts',(2.31142159057333,2.58116161377208,5.97815448255858));
#17252=CARTESIAN_POINT('Ctrl Pts',(2.36128434130696,2.56784999958469,5.93183474087357));
#17253=CARTESIAN_POINT('Ctrl Pts',(2.46729918759723,2.54332863292027,5.83885512810807));
#17254=CARTESIAN_POINT('Ctrl Pts',(2.56567273666995,2.53021793080961,5.72941144954258));
#17255=CARTESIAN_POINT('Ctrl Pts',(2.63596652889653,2.52334815894777,5.62089094351626));
#17256=CARTESIAN_POINT('Ctrl Pts',(2.68071920404472,2.52052866674434,5.52338620228086));
#17257=CARTESIAN_POINT('Ctrl Pts',(2.69557514809684,2.5200759873036,5.43965416929018));
#17258=CARTESIAN_POINT('Ctrl Pts',(2.69829980684391,2.52001806864527,5.40717967697245));
#17259=CARTESIAN_POINT('Ctrl Pts',(2.348995337768,2.58744107584805,6.01494078908319));
#17260=CARTESIAN_POINT('Ctrl Pts',(2.39865683979462,2.57856666638979,5.96728981679918));
#17261=CARTESIAN_POINT('Ctrl Pts',(2.50379036101454,2.56221908861351,5.86841726345666));
#17262=CARTESIAN_POINT('Ctrl Pts',(2.60032540397316,2.55347862053974,5.74988540376893));
#17263=CARTESIAN_POINT('Ctrl Pts',(2.66846922987872,2.54889877263185,5.63346263613916));
#17264=CARTESIAN_POINT('Ctrl Pts',(2.7110544394694,2.54701911116289,5.52956123521929));
#17265=CARTESIAN_POINT('Ctrl Pts',(2.72371676539789,2.54671732486907,5.44131770509742));
#17266=CARTESIAN_POINT('Ctrl Pts',(2.7255332045626,2.54667871243018,5.40717967697245));
#17267=CARTESIAN_POINT('Ctrl Pts',(2.38656908496267,2.59372053792403,6.05172709560779));
#17268=CARTESIAN_POINT('Ctrl Pts',(2.43602933828227,2.5892833331949,6.00274489272478));
#17269=CARTESIAN_POINT('Ctrl Pts',(2.54028153443185,2.58110954430676,5.89797939880525));
#17270=CARTESIAN_POINT('Ctrl Pts',(2.63497807127636,2.57673931026987,5.77035935799528));
#17271=CARTESIAN_POINT('Ctrl Pts',(2.70097193086091,2.57444938631592,5.64603432876207));
#17272=CARTESIAN_POINT('Ctrl Pts',(2.74138967489408,2.57350955558144,5.53573626815772));
#17273=CARTESIAN_POINT('Ctrl Pts',(2.75185838269895,2.57335866243453,5.44298124090466));
#17274=CARTESIAN_POINT('Ctrl Pts',(2.7527666022813,2.57333935621509,5.40717967697245));
#17275=CARTESIAN_POINT('Ctrl Pts',(2.42414283215735,2.6,6.0885134021324));
#17276=CARTESIAN_POINT('Ctrl Pts',(2.47340183676993,2.6,6.03819996865039));
#17277=CARTESIAN_POINT('Ctrl Pts',(2.57677270784915,2.6,5.92754153415384));
#17278=CARTESIAN_POINT('Ctrl Pts',(2.66963073857957,2.6,5.79083331222164));
#17279=CARTESIAN_POINT('Ctrl Pts',(2.7334746318431,2.6,5.65860602138498));
#17280=CARTESIAN_POINT('Ctrl Pts',(2.77172491031876,2.6,5.54191130109615));
#17281=CARTESIAN_POINT('Ctrl Pts',(2.78,2.6,5.44464477671191));
#17282=CARTESIAN_POINT('Ctrl Pts',(2.78,2.6,5.40717967697245));
#17283=CARTESIAN_POINT('',(2.31142159057333,2.58116161377208,5.97815448255858));
#17284=CARTESIAN_POINT('Ctrl Pts',(2.31142159057333,2.58116161377208,5.97815448255858));
#17285=CARTESIAN_POINT('Ctrl Pts',(2.348995337768,2.58744107584805,6.01494078908319));
#17286=CARTESIAN_POINT('Ctrl Pts',(2.38656908496267,2.59372053792403,6.05172709560779));
#17287=CARTESIAN_POINT('Ctrl Pts',(2.42414283215735,2.6,6.0885134021324));
#17288=CARTESIAN_POINT('Ctrl Pts',(2.69829980684391,2.52001806864527,5.40717967697245));
#17289=CARTESIAN_POINT('Ctrl Pts',(2.69557514809684,2.5200759873036,5.43965416929018));
#17290=CARTESIAN_POINT('Ctrl Pts',(2.68071920404472,2.52052866674434,5.52338620228086));
#17291=CARTESIAN_POINT('Ctrl Pts',(2.63596652889653,2.52334815894777,5.62089094351626));
#17292=CARTESIAN_POINT('Ctrl Pts',(2.56567273666995,2.53021793080961,5.72941144954258));
#17293=CARTESIAN_POINT('Ctrl Pts',(2.46729918759723,2.54332863292027,5.83885512810807));
#17294=CARTESIAN_POINT('Ctrl Pts',(2.36128434130696,2.56784999958469,5.93183474087357));
#17295=CARTESIAN_POINT('Ctrl Pts',(2.31142159057333,2.58116161377208,5.97815448255858));
#17296=CARTESIAN_POINT('Origin',(-2.74,0.,0.04));
#17297=CARTESIAN_POINT('Origin',(-5.71,0.,0.04));
#17298=CARTESIAN_POINT('Origin',(5.71,0.,0.04));
#17299=CARTESIAN_POINT('Origin',(2.74,0.,0.04));
#17300=CARTESIAN_POINT('Origin',(2.74,2.56,2.1875));
#17301=CARTESIAN_POINT('Origin',(-5.71,2.56,2.1875));
#17302=CARTESIAN_POINT('Origin',(-2.74,-2.56,5.0375));
#17303=CARTESIAN_POINT('Ctrl Pts',(2.69829980684391,-2.52001806864527,5.40717967697245));
#17304=CARTESIAN_POINT('Ctrl Pts',(2.69528352551617,-2.52008218638766,5.44312994227118));
#17305=CARTESIAN_POINT('Ctrl Pts',(2.68123989111592,-2.52051013648877,5.51729816380893));
#17306=CARTESIAN_POINT('Ctrl Pts',(2.63367794162332,-2.52356953989164,5.62595269195354));
#17307=CARTESIAN_POINT('Ctrl Pts',(2.55608221571234,-2.53094020120163,5.74414944732199));
#17308=CARTESIAN_POINT('Ctrl Pts',(2.47881891560007,-2.54263648495202,5.82345543387705));
#17309=CARTESIAN_POINT('Ctrl Pts',(2.38591323923068,-2.56211985755297,5.91035968403401));
#17310=CARTESIAN_POINT('Ctrl Pts',(2.34794220819964,-2.57141188347425,5.9442288456962));
#17311=CARTESIAN_POINT('Ctrl Pts',(2.31142159080892,-2.58116161370918,5.97815448233973));
#17312=CARTESIAN_POINT('Ctrl Pts',(2.7255332045626,-2.54667871243018,5.40717967697245));
#17313=CARTESIAN_POINT('Ctrl Pts',(2.72353019295656,-2.54670588833705,5.44500465970129));
#17314=CARTESIAN_POINT('Ctrl Pts',(2.71140788262801,-2.54701636077182,5.52317099586011));
#17315=CARTESIAN_POINT('Ctrl Pts',(2.66629357290831,-2.54905511343735,5.63884881308445));
#17316=CARTESIAN_POINT('Ctrl Pts',(2.59103946170864,-2.55395127036495,5.76578291819495));
#17317=CARTESIAN_POINT('Ctrl Pts',(2.51499306415409,-2.56181835630172,5.8516058289363));
#17318=CARTESIAN_POINT('Ctrl Pts',(2.4230785617572,-2.57470877665646,5.94444781460691));
#17319=CARTESIAN_POINT('Ctrl Pts',(2.38536381613614,-2.5809733210315,5.98001412068834));
#17320=CARTESIAN_POINT('Ctrl Pts',(2.34899533800264,-2.58744107580612,6.01494078885804));
#17321=CARTESIAN_POINT('Ctrl Pts',(2.7527666022813,-2.57333935621509,5.40717967697245));
#17322=CARTESIAN_POINT('Ctrl Pts',(2.75175333255962,-2.57337629805061,5.4467799812886));
#17323=CARTESIAN_POINT('Ctrl Pts',(2.7415821395726,-2.57349377571695,5.52908162910424));
#17324=CARTESIAN_POINT('Ctrl Pts',(2.6989137440639,-2.57451442645429,5.65177067977436));
#17325=CARTESIAN_POINT('Ctrl Pts',(2.62597409522993,-2.57698893083669,5.78730964038079));
#17326=CARTESIAN_POINT('Ctrl Pts',(2.55119649000168,-2.58081812865031,5.87997558417632));
#17327=CARTESIAN_POINT('Ctrl Pts',(2.4602196462861,-2.58741108089651,5.9783727139586));
#17328=CARTESIAN_POINT('Ctrl Pts',(2.42279964439558,-2.59043856244275,6.01587741917045));
#17329=CARTESIAN_POINT('Ctrl Pts',(2.38656908519636,-2.59372053790306,6.05172709537636));
#17330=CARTESIAN_POINT('Ctrl Pts',(2.78,-2.6,5.40717967697245));
#17331=CARTESIAN_POINT('Ctrl Pts',(2.78,-2.6,5.44865469871872));
#17332=CARTESIAN_POINT('Ctrl Pts',(2.77175013108469,-2.6,5.53495446115542));
#17333=CARTESIAN_POINT('Ctrl Pts',(2.73152937534889,-2.6,5.66466680090526));
#17334=CARTESIAN_POINT('Ctrl Pts',(2.66093134122623,-2.6,5.80894311125375));
#17335=CARTESIAN_POINT('Ctrl Pts',(2.5873706385557,-2.6,5.90812597923557));
#17336=CARTESIAN_POINT('Ctrl Pts',(2.49738496881261,-2.6,6.0124608445315));
#17337=CARTESIAN_POINT('Ctrl Pts',(2.46022125233207,-2.6,6.05166269416259));
#17338=CARTESIAN_POINT('Ctrl Pts',(2.42414283239008,-2.6,6.08851340189468));
#17339=CARTESIAN_POINT('',(2.31142159080892,-2.58116161370918,5.97815448233973));
#17340=CARTESIAN_POINT('Ctrl Pts',(2.42414283239008,-2.6,6.08851340189468));
#17341=CARTESIAN_POINT('Ctrl Pts',(2.38656908519636,-2.59372053790306,6.05172709537636));
#17342=CARTESIAN_POINT('Ctrl Pts',(2.34899533800264,-2.58744107580612,6.01494078885804));
#17343=CARTESIAN_POINT('Ctrl Pts',(2.31142159080892,-2.58116161370918,5.97815448233973));
#17344=CARTESIAN_POINT('',(2.69829980684391,-2.52001806864527,5.40717967697245));
#17345=CARTESIAN_POINT('Ctrl Pts',(2.31142159080892,-2.58116161370918,5.97815448233973));
#17346=CARTESIAN_POINT('Ctrl Pts',(2.34794220819964,-2.57141188347425,5.9442288456962));
#17347=CARTESIAN_POINT('Ctrl Pts',(2.38591323923068,-2.56211985755297,5.91035968403401));
#17348=CARTESIAN_POINT('Ctrl Pts',(2.47881891560007,-2.54263648495202,5.82345543387705));
#17349=CARTESIAN_POINT('Ctrl Pts',(2.55608221571234,-2.53094020120163,5.74414944732199));
#17350=CARTESIAN_POINT('Ctrl Pts',(2.63367794162332,-2.52356953989164,5.62595269195354));
#17351=CARTESIAN_POINT('Ctrl Pts',(2.68123989111592,-2.52051013648877,5.51729816380893));
#17352=CARTESIAN_POINT('Ctrl Pts',(2.69528352551617,-2.52008218638766,5.44312994227118));
#17353=CARTESIAN_POINT('Ctrl Pts',(2.69829980684391,-2.52001806864527,5.40717967697245));
#17354=CARTESIAN_POINT('',(2.69829980684391,-2.52001806864527,5.40717967697245));
#17355=CARTESIAN_POINT('Ctrl Pts',(2.7,-2.52,5.36678788880707));
#17356=CARTESIAN_POINT('Ctrl Pts',(2.7,-2.52,5.38025181819553));
#17357=CARTESIAN_POINT('Ctrl Pts',(2.69942945076934,-2.51999405556084,5.39371574758399));
#17358=CARTESIAN_POINT('Ctrl Pts',(2.69829980684391,-2.52001806864527,5.40717967697245));
#17359=CARTESIAN_POINT('Ctrl Pts',(2.72666666666667,-2.54666666666667,5.36678788880707));
#17360=CARTESIAN_POINT('Ctrl Pts',(2.72666666666667,-2.54666666666667,5.38025181819553));
#17361=CARTESIAN_POINT('Ctrl Pts',(2.72628630051289,-2.54666270370723,5.39371574758399));
#17362=CARTESIAN_POINT('Ctrl Pts',(2.7255332045626,-2.54667871243018,5.40717967697245));
#17363=CARTESIAN_POINT('Ctrl Pts',(2.75333333333333,-2.57333333333333,5.36678788880707));
#17364=CARTESIAN_POINT('Ctrl Pts',(2.75333333333333,-2.57333333333333,5.38025181819553));
#17365=CARTESIAN_POINT('Ctrl Pts',(2.75314315025645,-2.57333135185361,5.39371574758399));
#17366=CARTESIAN_POINT('Ctrl Pts',(2.7527666022813,-2.57333935621509,5.40717967697245));
#17367=CARTESIAN_POINT('Ctrl Pts',(2.78,-2.6,5.36678788880707));
#17368=CARTESIAN_POINT('Ctrl Pts',(2.78,-2.6,5.38025181819553));
#17369=CARTESIAN_POINT('Ctrl Pts',(2.78,-2.6,5.39371574758399));
#17370=CARTESIAN_POINT('Ctrl Pts',(2.78,-2.6,5.40717967697245));
#17371=CARTESIAN_POINT('Ctrl Pts',(2.69829980684391,-2.52001806864527,5.40717967697245));
#17372=CARTESIAN_POINT('Ctrl Pts',(2.69942945076934,-2.51999405556084,5.39371574758399));
#17373=CARTESIAN_POINT('Ctrl Pts',(2.7,-2.52,5.38025181819553));
#17374=CARTESIAN_POINT('Ctrl Pts',(2.7,-2.52,5.36678788880707));
#17375=CARTESIAN_POINT('Ctrl Pts',(-2.69829980684391,2.52001806864527,5.40717967697245));
#17376=CARTESIAN_POINT('Ctrl Pts',(-2.69528352551617,2.52008218638766,5.44312994227118));
#17377=CARTESIAN_POINT('Ctrl Pts',(-2.68123989111592,2.52051013648877,5.51729816380893));
#17378=CARTESIAN_POINT('Ctrl Pts',(-2.63367794162332,2.52356953989164,5.62595269195354));
#17379=CARTESIAN_POINT('Ctrl Pts',(-2.55608221571234,2.53094020120163,5.744149447322));
#17380=CARTESIAN_POINT('Ctrl Pts',(-2.47881891560007,2.54263648495202,5.82345543387705));
#17381=CARTESIAN_POINT('Ctrl Pts',(-2.38591323923047,2.56211985755302,5.91035968403422));
#17382=CARTESIAN_POINT('Ctrl Pts',(-2.34794220819919,2.57141188347436,5.9442288456966));
#17383=CARTESIAN_POINT('Ctrl Pts',(-2.31142159080827,2.58116161370936,5.97815448234033));
#17384=CARTESIAN_POINT('Ctrl Pts',(-2.7255332045626,2.54667871243018,5.40717967697245));
#17385=CARTESIAN_POINT('Ctrl Pts',(-2.72353019295656,2.54670588833705,5.44500465970129));
#17386=CARTESIAN_POINT('Ctrl Pts',(-2.71140788262801,2.54701636077182,5.52317099586011));
#17387=CARTESIAN_POINT('Ctrl Pts',(-2.66629357290831,2.54905511343735,5.63884881308445));
#17388=CARTESIAN_POINT('Ctrl Pts',(-2.59103946170864,2.55395127036495,5.76578291819496));
#17389=CARTESIAN_POINT('Ctrl Pts',(-2.51499306415409,2.56181835630172,5.8516058289363));
#17390=CARTESIAN_POINT('Ctrl Pts',(-2.42307856175698,2.5747087766565,5.94444781460713));
#17391=CARTESIAN_POINT('Ctrl Pts',(-2.38536381613569,2.58097332103158,5.98001412068877));
#17392=CARTESIAN_POINT('Ctrl Pts',(-2.34899533800199,2.58744107580624,6.01494078885867));
#17393=CARTESIAN_POINT('Ctrl Pts',(-2.7527666022813,2.57333935621509,5.40717967697245));
#17394=CARTESIAN_POINT('Ctrl Pts',(-2.75175333255962,2.57337629805061,5.4467799812886));
#17395=CARTESIAN_POINT('Ctrl Pts',(-2.74158213957261,2.57349377571695,5.52908162910424));
#17396=CARTESIAN_POINT('Ctrl Pts',(-2.69891374406391,2.57451442645429,5.65177067977436));
#17397=CARTESIAN_POINT('Ctrl Pts',(-2.62597409522993,2.57698893083669,5.78730964038079));
#17398=CARTESIAN_POINT('Ctrl Pts',(-2.55119649000168,2.58081812865031,5.87997558417632));
#17399=CARTESIAN_POINT('Ctrl Pts',(-2.46021964628589,2.58741108089653,5.97837271395883));
#17400=CARTESIAN_POINT('Ctrl Pts',(-2.42279964439514,2.59043856244278,6.01587741917089));
#17401=CARTESIAN_POINT('Ctrl Pts',(-2.38656908519572,2.59372053790312,6.051727095377));
#17402=CARTESIAN_POINT('Ctrl Pts',(-2.78,2.6,5.40717967697245));
#17403=CARTESIAN_POINT('Ctrl Pts',(-2.78,2.6,5.44865469871872));
#17404=CARTESIAN_POINT('Ctrl Pts',(-2.77175013108469,2.6,5.53495446115542));
#17405=CARTESIAN_POINT('Ctrl Pts',(-2.7315293753489,2.6,5.66466680090526));
#17406=CARTESIAN_POINT('Ctrl Pts',(-2.66093134122624,2.6,5.80894311125375));
#17407=CARTESIAN_POINT('Ctrl Pts',(-2.5873706385557,2.6,5.90812597923557));
#17408=CARTESIAN_POINT('Ctrl Pts',(-2.4973849688124,2.6,6.01246084453175));
#17409=CARTESIAN_POINT('Ctrl Pts',(-2.46022125233163,2.6,6.05166269416306));
#17410=CARTESIAN_POINT('Ctrl Pts',(-2.42414283238944,2.6,6.08851340189533));
#17411=CARTESIAN_POINT('',(-2.31142159080827,2.58116161370936,5.97815448234033));
#17412=CARTESIAN_POINT('Ctrl Pts',(-2.42414283238944,2.6,6.08851340189533));
#17413=CARTESIAN_POINT('Ctrl Pts',(-2.38656908519572,2.59372053790312,6.051727095377));
#17414=CARTESIAN_POINT('Ctrl Pts',(-2.34899533800199,2.58744107580624,6.01494078885867));
#17415=CARTESIAN_POINT('Ctrl Pts',(-2.31142159080827,2.58116161370936,5.97815448234033));
#17416=CARTESIAN_POINT('',(-2.69829980684391,2.52001806864527,5.40717967697245));
#17417=CARTESIAN_POINT('Ctrl Pts',(-2.31142159080827,2.58116161370936,5.97815448234033));
#17418=CARTESIAN_POINT('Ctrl Pts',(-2.34794220819919,2.57141188347436,5.9442288456966));
#17419=CARTESIAN_POINT('Ctrl Pts',(-2.38591323923047,2.56211985755302,5.91035968403422));
#17420=CARTESIAN_POINT('Ctrl Pts',(-2.47881891560007,2.54263648495202,5.82345543387705));
#17421=CARTESIAN_POINT('Ctrl Pts',(-2.55608221571234,2.53094020120163,5.744149447322));
#17422=CARTESIAN_POINT('Ctrl Pts',(-2.63367794162332,2.52356953989164,5.62595269195354));
#17423=CARTESIAN_POINT('Ctrl Pts',(-2.68123989111592,2.52051013648877,5.51729816380893));
#17424=CARTESIAN_POINT('Ctrl Pts',(-2.69528352551617,2.52008218638766,5.44312994227118));
#17425=CARTESIAN_POINT('Ctrl Pts',(-2.69829980684391,2.52001806864527,5.40717967697245));
#17426=CARTESIAN_POINT('',(-2.69829980684391,2.52001806864527,5.40717967697245));
#17427=CARTESIAN_POINT('Ctrl Pts',(-2.7,2.52,5.36678788880707));
#17428=CARTESIAN_POINT('Ctrl Pts',(-2.7,2.52,5.38025181819553));
#17429=CARTESIAN_POINT('Ctrl Pts',(-2.69942945076934,2.51999405556084,5.39371574758399));
#17430=CARTESIAN_POINT('Ctrl Pts',(-2.69829980684391,2.52001806864527,5.40717967697245));
#17431=CARTESIAN_POINT('Ctrl Pts',(-2.72666666666667,2.54666666666667,5.36678788880707));
#17432=CARTESIAN_POINT('Ctrl Pts',(-2.72666666666667,2.54666666666667,5.38025181819553));
#17433=CARTESIAN_POINT('Ctrl Pts',(-2.72628630051289,2.54666270370723,5.39371574758399));
#17434=CARTESIAN_POINT('Ctrl Pts',(-2.7255332045626,2.54667871243018,5.40717967697245));
#17435=CARTESIAN_POINT('Ctrl Pts',(-2.75333333333333,2.57333333333333,5.36678788880707));
#17436=CARTESIAN_POINT('Ctrl Pts',(-2.75333333333333,2.57333333333333,5.38025181819553));
#17437=CARTESIAN_POINT('Ctrl Pts',(-2.75314315025645,2.57333135185361,5.39371574758399));
#17438=CARTESIAN_POINT('Ctrl Pts',(-2.7527666022813,2.57333935621509,5.40717967697245));
#17439=CARTESIAN_POINT('Ctrl Pts',(-2.78,2.6,5.36678788880707));
#17440=CARTESIAN_POINT('Ctrl Pts',(-2.78,2.6,5.38025181819553));
#17441=CARTESIAN_POINT('Ctrl Pts',(-2.78,2.6,5.39371574758399));
#17442=CARTESIAN_POINT('Ctrl Pts',(-2.78,2.6,5.40717967697245));
#17443=CARTESIAN_POINT('Ctrl Pts',(-2.69829980684391,2.52001806864527,5.40717967697245));
#17444=CARTESIAN_POINT('Ctrl Pts',(-2.69942945076934,2.51999405556084,5.39371574758399));
#17445=CARTESIAN_POINT('Ctrl Pts',(-2.7,2.52,5.38025181819553));
#17446=CARTESIAN_POINT('Ctrl Pts',(-2.7,2.52,5.36678788880707));
#17447=CARTESIAN_POINT('Ctrl Pts',(-2.31142159057266,-2.58116161377225,
5.9781544825592));
#17448=CARTESIAN_POINT('Ctrl Pts',(-2.30761542875944,-2.59362449027802,
6.01749838383513));
#17449=CARTESIAN_POINT('Ctrl Pts',(-2.30380771440082,-2.6,6.05874632271281));
#17450=CARTESIAN_POINT('Ctrl Pts',(-2.3,-2.6,6.1));
#17451=CARTESIAN_POINT('Ctrl Pts',(-2.34899533776733,-2.58744107584817,
6.01494078908382));
#17452=CARTESIAN_POINT('Ctrl Pts',(-2.33266424854111,-2.59574966018535,
6.04244634525299));
#17453=CARTESIAN_POINT('Ctrl Pts',(-2.31633212428463,-2.6,6.07122125982333));
#17454=CARTESIAN_POINT('Ctrl Pts',(-2.3,-2.6,6.1));
#17455=CARTESIAN_POINT('Ctrl Pts',(-2.38656908496201,-2.59372053792408,
6.05172709560844));
#17456=CARTESIAN_POINT('Ctrl Pts',(-2.35771306832278,-2.59787483009267,
6.06739430667085));
#17457=CARTESIAN_POINT('Ctrl Pts',(-2.32885653416843,-2.6,6.08369619693384));
#17458=CARTESIAN_POINT('Ctrl Pts',(-2.3,-2.6,6.1));
#17459=CARTESIAN_POINT('Ctrl Pts',(-2.42414283215669,-2.6,6.08851340213307));
#17460=CARTESIAN_POINT('Ctrl Pts',(-2.38276188810446,-2.6,6.09234226808871));
#17461=CARTESIAN_POINT('Ctrl Pts',(-2.34138094405223,-2.6,6.09617113404436));
#17462=CARTESIAN_POINT('Ctrl Pts',(-2.3,-2.6,6.1));
#17463=CARTESIAN_POINT('Ctrl Pts',(-2.31142159057266,-2.58116161377225,
5.9781544825592));
#17464=CARTESIAN_POINT('Ctrl Pts',(-2.30761542875944,-2.59362449027802,
6.01749838383513));
#17465=CARTESIAN_POINT('Ctrl Pts',(-2.30380771440082,-2.6,6.05874632271281));
#17466=CARTESIAN_POINT('Ctrl Pts',(-2.3,-2.6,6.1));
#17467=CARTESIAN_POINT('Ctrl Pts',(2.31142159057333,2.58116161377208,5.97815448255858));
#17468=CARTESIAN_POINT('Ctrl Pts',(2.30761542875988,2.59362449027796,6.0174983838347));
#17469=CARTESIAN_POINT('Ctrl Pts',(2.30380771440105,2.6,6.0587463227126));
#17470=CARTESIAN_POINT('Ctrl Pts',(2.3,2.6,6.1));
#17471=CARTESIAN_POINT('Ctrl Pts',(2.348995337768,2.58744107584805,6.01494078908319));
#17472=CARTESIAN_POINT('Ctrl Pts',(2.33266424854156,2.59574966018531,6.04244634525256));
#17473=CARTESIAN_POINT('Ctrl Pts',(2.31633212428485,2.6,6.07122125982311));
#17474=CARTESIAN_POINT('Ctrl Pts',(2.3,2.6,6.1));
#17475=CARTESIAN_POINT('Ctrl Pts',(2.38656908496267,2.59372053792403,6.05172709560779));
#17476=CARTESIAN_POINT('Ctrl Pts',(2.35771306832323,2.59787483009265,6.06739430667041));
#17477=CARTESIAN_POINT('Ctrl Pts',(2.32885653416865,2.6,6.08369619693362));
#17478=CARTESIAN_POINT('Ctrl Pts',(2.3,2.6,6.1));
#17479=CARTESIAN_POINT('Ctrl Pts',(2.42414283215735,2.6,6.0885134021324));
#17480=CARTESIAN_POINT('Ctrl Pts',(2.3827618881049,2.6,6.09234226808826));
#17481=CARTESIAN_POINT('Ctrl Pts',(2.34138094405245,2.6,6.09617113404413));
#17482=CARTESIAN_POINT('Ctrl Pts',(2.3,2.6,6.1));
#17483=CARTESIAN_POINT('Ctrl Pts',(2.31142159057333,2.58116161377208,5.97815448255858));
#17484=CARTESIAN_POINT('Ctrl Pts',(2.30761542875988,2.59362449027796,6.0174983838347));
#17485=CARTESIAN_POINT('Ctrl Pts',(2.30380771440105,2.6,6.0587463227126));
#17486=CARTESIAN_POINT('Ctrl Pts',(2.3,2.6,6.1));
#17487=CARTESIAN_POINT('Ctrl Pts',(2.42414283239008,-2.6,6.08851340189468));
#17488=CARTESIAN_POINT('Ctrl Pts',(2.38276188826005,-2.6,6.09234226792978));
#17489=CARTESIAN_POINT('Ctrl Pts',(2.34138094413003,-2.6,6.09617113396489));
#17490=CARTESIAN_POINT('Ctrl Pts',(2.3,-2.6,6.1));
#17491=CARTESIAN_POINT('Ctrl Pts',(2.38656908519636,-2.59372053790306,6.05172709537636));
#17492=CARTESIAN_POINT('Ctrl Pts',(2.35771306847904,-2.59787483008549,6.06739430651421));
#17493=CARTESIAN_POINT('Ctrl Pts',(2.32885653424655,-2.6,6.08369619685551));
#17494=CARTESIAN_POINT('Ctrl Pts',(2.3,-2.6,6.1));
#17495=CARTESIAN_POINT('Ctrl Pts',(2.34899533800264,-2.58744107580612,6.01494078885804));
#17496=CARTESIAN_POINT('Ctrl Pts',(2.33266424869802,-2.59574966017099,6.04244634509863));
#17497=CARTESIAN_POINT('Ctrl Pts',(2.31633212436308,-2.6,6.07122125974614));
#17498=CARTESIAN_POINT('Ctrl Pts',(2.3,-2.6,6.1));
#17499=CARTESIAN_POINT('Ctrl Pts',(2.31142159080892,-2.58116161370918,5.97815448233973));
#17500=CARTESIAN_POINT('Ctrl Pts',(2.30761542891701,-2.59362449025648,6.01749838368306));
#17501=CARTESIAN_POINT('Ctrl Pts',(2.30380771447961,-2.6,6.05874632263676));
#17502=CARTESIAN_POINT('Ctrl Pts',(2.3,-2.6,6.1));
#17503=CARTESIAN_POINT('Ctrl Pts',(2.3,-2.6,6.1));
#17504=CARTESIAN_POINT('Ctrl Pts',(2.30380771447961,-2.6,6.05874632263676));
#17505=CARTESIAN_POINT('Ctrl Pts',(2.30761542891701,-2.59362449025648,6.01749838368306));
#17506=CARTESIAN_POINT('Ctrl Pts',(2.31142159080892,-2.58116161370918,5.97815448233973));
#17507=CARTESIAN_POINT('Ctrl Pts',(-2.42414283238944,2.6,6.08851340189533));
#17508=CARTESIAN_POINT('Ctrl Pts',(-2.38276188825963,2.6,6.09234226793022));
#17509=CARTESIAN_POINT('Ctrl Pts',(-2.34138094412981,2.6,6.09617113396511));
#17510=CARTESIAN_POINT('Ctrl Pts',(-2.3,2.6,6.1));
#17511=CARTESIAN_POINT('Ctrl Pts',(-2.38656908519572,2.59372053790312,6.051727095377));
#17512=CARTESIAN_POINT('Ctrl Pts',(-2.35771306847861,2.59787483008551,6.06739430651464));
#17513=CARTESIAN_POINT('Ctrl Pts',(-2.32885653424634,2.6,6.08369619685573));
#17514=CARTESIAN_POINT('Ctrl Pts',(-2.3,2.6,6.1));
#17515=CARTESIAN_POINT('Ctrl Pts',(-2.34899533800199,2.58744107580624,6.01494078885867));
#17516=CARTESIAN_POINT('Ctrl Pts',(-2.33266424869759,2.59574966017103,6.04244634509906));
#17517=CARTESIAN_POINT('Ctrl Pts',(-2.31633212436287,2.6,6.07122125974635));
#17518=CARTESIAN_POINT('Ctrl Pts',(-2.3,2.6,6.1));
#17519=CARTESIAN_POINT('Ctrl Pts',(-2.31142159080827,2.58116161370936,5.97815448234033));
#17520=CARTESIAN_POINT('Ctrl Pts',(-2.30761542891658,2.59362449025654,6.01749838368348));
#17521=CARTESIAN_POINT('Ctrl Pts',(-2.30380771447939,2.6,6.05874632263697));
#17522=CARTESIAN_POINT('Ctrl Pts',(-2.3,2.6,6.1));
#17523=CARTESIAN_POINT('Ctrl Pts',(-2.3,2.6,6.1));
#17524=CARTESIAN_POINT('Ctrl Pts',(-2.30380771447939,2.6,6.05874632263697));
#17525=CARTESIAN_POINT('Ctrl Pts',(-2.30761542891658,2.59362449025654,6.01749838368348));
#17526=CARTESIAN_POINT('Ctrl Pts',(-2.31142159080827,2.58116161370936,5.97815448234033));
#17527=CARTESIAN_POINT('Origin',(-2.3,-2.2,6.1));
#17528=CARTESIAN_POINT('',(-2.3,-2.2,5.7));
#17529=CARTESIAN_POINT('Origin',(-2.3,-2.2,5.3));
#17530=CARTESIAN_POINT('Origin',(-2.3,-2.2,6.1));
#17531=CARTESIAN_POINT('Origin',(-2.3,2.2,6.1));
#17532=CARTESIAN_POINT('',(-2.3,2.2,5.7));
#17533=CARTESIAN_POINT('Origin',(-2.3,2.2,6.1));
#17534=CARTESIAN_POINT('Origin',(-2.3,2.2,5.3));
#17535=CARTESIAN_POINT('Origin',(-5.75,0.,8.75));
#17536=CARTESIAN_POINT('Origin',(2.3,2.2,6.1));
#17537=CARTESIAN_POINT('',(2.3,2.2,5.7));
#17538=CARTESIAN_POINT('Origin',(2.3,2.2,5.3));
#17539=CARTESIAN_POINT('Origin',(2.3,2.2,6.1));
#17540=CARTESIAN_POINT('Origin',(2.3,0.,5.3));
#17541=CARTESIAN_POINT('',(2.3,-2.2,5.7));
#17542=CARTESIAN_POINT('Origin',(2.3,-2.2,5.3));
#17543=CARTESIAN_POINT('',(2.3,0.,5.7));
#17544=CARTESIAN_POINT('Origin',(2.3,-2.2,6.1));
#17545=CARTESIAN_POINT('Origin',(2.3,-2.2,6.1));
#17546=CARTESIAN_POINT('Origin',(-2.3,0.,5.3));
#17547=CARTESIAN_POINT('',(-2.3,0.,5.7));
#17548=CARTESIAN_POINT('Origin',(1.35,2.2,6.1));
#17549=CARTESIAN_POINT('',(1.35,2.2,5.7));
#17550=CARTESIAN_POINT('Origin',(2.7,0.,5.7));
#17551=CARTESIAN_POINT('',(1.35,-2.2,5.7));
#17552=CARTESIAN_POINT('Origin',(1.35,-2.2,6.1));
#17553=CARTESIAN_POINT('',(0.,0.,0.));
#17554=CARTESIAN_POINT('Origin',(0.,-4.39450830404517E-17,2.08232233047034));
#17555=CARTESIAN_POINT('',(1.35,-1.65327317884893E-16,2.1));
#17556=CARTESIAN_POINT('Origin',(0.,0.,2.1));
#17557=CARTESIAN_POINT('',(1.43535533905933,1.75780332161807E-16,2.06464466094067));
#17558=CARTESIAN_POINT('',(1.39267766952966,1.7055382502335E-16,2.08232233047034));
#17559=CARTESIAN_POINT('',(-1.43535533905933,-1.75780332161807E-16,2.06464466094067));
#17560=CARTESIAN_POINT('Origin',(0.,-8.78901660809035E-17,2.06464466094067));
#17561=CARTESIAN_POINT('Origin',(0.,-8.78901660809035E-17,2.06464466094067));
#17562=CARTESIAN_POINT('Origin',(0.,0.,1.86807790411448));
#17563=CARTESIAN_POINT('',(-1.82153560215913,6.70435414410743E-13,1.67846439784087));
#17564=CARTESIAN_POINT('',(-1.63192209588552,-1.99852817118404E-16,1.86807790411448));
#17565=CARTESIAN_POINT('',(-1.58980227845634,-0.0690572297370878,1.90869858745619));
#17566=CARTESIAN_POINT('Ctrl Pts',(-1.82153560215913,1.34132982498869E-12,
1.67846439784087));
#17567=CARTESIAN_POINT('Ctrl Pts',(-1.79844488399902,-0.0142452763777164,
1.70155511600098));
#17568=CARTESIAN_POINT('Ctrl Pts',(-1.77621769100022,-0.0263518482108029,
1.7236179719196));
#17569=CARTESIAN_POINT('Ctrl Pts',(-1.73494412567812,-0.0458782640980182,
1.76447740749199));
#17570=CARTESIAN_POINT('Ctrl Pts',(-1.70513299984439,-0.0588876017641377,
1.79387050688965));
#17571=CARTESIAN_POINT('Ctrl Pts',(-1.65153927195835,-0.0709952547837174,
1.84694613619239));
#17572=CARTESIAN_POINT('Ctrl Pts',(-1.62431631612136,-0.0738960377458574,
1.87400707649559));
#17573=CARTESIAN_POINT('Ctrl Pts',(-1.58980227845634,-0.0690572297370876,
1.90869858745619));
#17574=CARTESIAN_POINT('',(-1.5699559447672,-0.259766273896473,1.90869858745619));
#17575=CARTESIAN_POINT('Ctrl Pts',(-1.58980227845634,-0.0690572297370881,
1.90869858745619));
#17576=CARTESIAN_POINT('Ctrl Pts',(-1.58741971380287,-0.10016208146902,
1.90972905962805));
#17577=CARTESIAN_POINT('Ctrl Pts',(-1.58467291856134,-0.131250509699782,
1.91020759537532));
#17578=CARTESIAN_POINT('Ctrl Pts',(-1.58148476202963,-0.162313364909724,
1.91020766105751));
#17579=CARTESIAN_POINT('Ctrl Pts',(-1.57814413491694,-0.194861771890304,
1.91020772988089));
#17580=CARTESIAN_POINT('Ctrl Pts',(-1.57432303476077,-0.227345240254554,
1.90968253191571));
#17581=CARTESIAN_POINT('Ctrl Pts',(-1.5699559447672,-0.259766273896472,
1.90869858745619));
#17582=CARTESIAN_POINT('',(-1.81394816223928,-0.428377445609996,1.63615580822897));
#17583=CARTESIAN_POINT('Ctrl Pts',(-1.5699559447672,-0.259766273896473,
1.90869858745619));
#17584=CARTESIAN_POINT('Ctrl Pts',(-1.61720542751897,-0.262319849600338,
1.86166605258312));
#17585=CARTESIAN_POINT('Ctrl Pts',(-1.6527385648653,-0.277648859152455,
1.82419649030025));
#17586=CARTESIAN_POINT('Ctrl Pts',(-1.72174825233757,-0.325349196383375,
1.74786428230184));
#17587=CARTESIAN_POINT('Ctrl Pts',(-1.76741714130056,-0.365195041946486,
1.69596272615694));
#17588=CARTESIAN_POINT('Ctrl Pts',(-1.81394816223928,-0.428377445609996,
1.63615580822897));
#17589=CARTESIAN_POINT('',(-1.78098192700405,-0.549562141057365,1.63615580822897));
#17590=CARTESIAN_POINT('Origin',(0.,0.,1.63615580822897));
#17591=CARTESIAN_POINT('',(-1.49065195897357,-0.55695325007777,1.90869858745619));
#17592=CARTESIAN_POINT('Ctrl Pts',(-1.78098192700405,-0.549562141057365,
1.63615580822897));
#17593=CARTESIAN_POINT('Ctrl Pts',(-1.73615378095071,-0.563182934028249,
1.67497485013899));
#17594=CARTESIAN_POINT('Ctrl Pts',(-1.69503929836625,-0.572158425678775,
1.71107791524196));
#17595=CARTESIAN_POINT('Ctrl Pts',(-1.63585275285353,-0.579760041152499,
1.76447740749373));
#17596=CARTESIAN_POINT('Ctrl Pts',(-1.60348058094793,-0.582920512008146,
1.79387050689049));
#17597=CARTESIAN_POINT('Ctrl Pts',(-1.54876844626294,-0.577874201600641,
1.84694613619458));
#17598=CARTESIAN_POINT('Ctrl Pts',(-1.52198148548954,-0.572220654147733,
1.87400707649755));
#17599=CARTESIAN_POINT('Ctrl Pts',(-1.49065195897357,-0.55695325007777,
1.90869858745619));
#17600=CARTESIAN_POINT('',(-1.41284463836769,-0.732195474855993,1.90869858745619));
#17601=CARTESIAN_POINT('Ctrl Pts',(-1.49065195897357,-0.556953250077769,
1.90869858745619));
#17602=CARTESIAN_POINT('Ctrl Pts',(-1.47877407754171,-0.585799469037713,
1.90972905962805));
#17603=CARTESIAN_POINT('Ctrl Pts',(-1.4665548673766,-0.614517514878265,
1.91020759537532));
#17604=CARTESIAN_POINT('Ctrl Pts',(-1.45392380017848,-0.643074851191362,
1.91020766105751));
#17605=CARTESIAN_POINT('Ctrl Pts',(-1.44068866409761,-0.672997915195582,
1.91020772988089));
#17606=CARTESIAN_POINT('Ctrl Pts',(-1.42701663813388,-0.702710744569809,
1.90968253191571));
#17607=CARTESIAN_POINT('Ctrl Pts',(-1.41284463836769,-0.732195474855993,
1.90869858745619));
#17608=CARTESIAN_POINT('',(-1.59279130921887,-0.967951970128403,1.63615580822897));
#17609=CARTESIAN_POINT('Ctrl Pts',(-1.41284463836769,-0.732195474855993,
1.90869858745619));
#17610=CARTESIAN_POINT('Ctrl Pts',(-1.45699246854074,-0.74922496281447,
1.86166605258385));
#17611=CARTESIAN_POINT('Ctrl Pts',(-1.48604956590001,-0.774784060540386,
1.82419649030103));
#17612=CARTESIAN_POINT('Ctrl Pts',(-1.53694146401283,-0.841474943294401,
1.74786428230768));
#17613=CARTESIAN_POINT('Ctrl Pts',(-1.56806211502062,-0.893483057166951,
1.69596272616206));
#17614=CARTESIAN_POINT('Ctrl Pts',(-1.59279130921887,-0.967951970128403,
1.63615580822897));
#17615=CARTESIAN_POINT('',(-1.5239904260293,-1.07301833748062,1.63615580822897));
#17616=CARTESIAN_POINT('Origin',(0.,0.,1.63615580822897));
#17617=CARTESIAN_POINT('',(-1.24558623976356,-0.990330805779365,1.90869858745619));
#17618=CARTESIAN_POINT('Ctrl Pts',(-1.5239904260293,-1.07301833748062,1.63615580822897));
#17619=CARTESIAN_POINT('Ctrl Pts',(-1.47714726910887,-1.07211982243591,
1.67497485013742));
#17620=CARTESIAN_POINT('Ctrl Pts',(-1.43527149308025,-1.06795094842396,
1.71107791523994));
#17621=CARTESIAN_POINT('Ctrl Pts',(-1.37663271492071,-1.05689086595159,
1.76447740749771));
#17622=CARTESIAN_POINT('Ctrl Pts',(-1.34486831068169,-1.04989310109001,
1.79387050689188));
#17623=CARTESIAN_POINT('Ctrl Pts',(-1.29439337414606,-1.02818679527844,
1.8469461361937));
#17624=CARTESIAN_POINT('Ctrl Pts',(-1.27066450279186,-1.01453232602662,
1.87400707649691));
#17625=CARTESIAN_POINT('Ctrl Pts',(-1.24558623976356,-0.990330805779365,
1.90869858745619));
#17626=CARTESIAN_POINT('',(-1.11743425489732,-1.13295228123076,1.90869858745619));
#17627=CARTESIAN_POINT('Ctrl Pts',(-1.24558623976356,-0.990330805779365,
1.90869858745619));
#17628=CARTESIAN_POINT('Ctrl Pts',(-1.22537573134593,-1.01409472307207,
1.90972905962805));
#17629=CARTESIAN_POINT('Ctrl Pts',(-1.20488020768447,-1.03763126410513,
1.91020759537532));
#17630=CARTESIAN_POINT('Ctrl Pts',(-1.18404264668309,-1.06088769047244,
1.91020766105751));
#17631=CARTESIAN_POINT('Ctrl Pts',(-1.16220854896825,-1.08525633350931,
1.91020772988089));
#17632=CARTESIAN_POINT('Ctrl Pts',(-1.14002391035689,-1.1092900251329,1.90968253191571));
#17633=CARTESIAN_POINT('Ctrl Pts',(-1.11743425489732,-1.13295228123076,
1.90869858745619));
#17634=CARTESIAN_POINT('',(-1.21572094522251,-1.4127766116927,1.63615580822897));
#17635=CARTESIAN_POINT('Ctrl Pts',(-1.11743425489733,-1.13295228123076,
1.90869858745619));
#17636=CARTESIAN_POINT('Ctrl Pts',(-1.15415893527728,-1.16279071650968,
1.86166605258608));
#17637=CARTESIAN_POINT('Ctrl Pts',(-1.17389568150815,-1.19607799984267,
1.82419649030342));
#17638=CARTESIAN_POINT('Ctrl Pts',(-1.20168813669714,-1.27523125986505,
1.74786428230159));
#17639=CARTESIAN_POINT('Ctrl Pts',(-1.21521424359529,-1.33431072550216,
1.69596272615648));
#17640=CARTESIAN_POINT('Ctrl Pts',(-1.21572094522251,-1.4127766116927,1.63615580822897));
#17641=CARTESIAN_POINT('',(-1.11782012388912,-1.4914400228729,1.63615580822897));
#17642=CARTESIAN_POINT('Origin',(0.,0.,1.63615580822897));
#17643=CARTESIAN_POINT('',(-0.878593860895847,-1.32676788217082,1.90869858745619));
#17644=CARTESIAN_POINT('Ctrl Pts',(-1.11782012388912,-1.4914400228729,1.63615580822897));
#17645=CARTESIAN_POINT('Ctrl Pts',(-1.07354729067195,-1.47611015272513,
1.67497485013978));
#17646=CARTESIAN_POINT('Ctrl Pts',(-1.03500931392296,-1.45920499148488,
1.71107791524182));
#17647=CARTESIAN_POINT('Ctrl Pts',(-0.982658275295231,-1.43056584900102,
1.76447740749414));
#17648=CARTESIAN_POINT('Ctrl Pts',(-0.954610959919589,-1.41409483840259,
1.79387050689094));
#17649=CARTESIAN_POINT('Ctrl Pts',(-0.913314059997475,-1.37785330163525,
1.84694613619429));
#17650=CARTESIAN_POINT('Ctrl Pts',(-0.894966025319891,-1.35753450517084,
1.87400707649751));
#17651=CARTESIAN_POINT('Ctrl Pts',(-0.878593860895848,-1.32676788217082,
1.90869858745619));
#17652=CARTESIAN_POINT('',(-0.712641620935351,-1.42280782457595,1.90869858745619));
#17653=CARTESIAN_POINT('Ctrl Pts',(-0.878593860895848,-1.32676788217082,
1.90869858745619));
#17654=CARTESIAN_POINT('Ctrl Pts',(-0.852029070871246,-1.34312331999875,
1.90972905962805));
#17655=CARTESIAN_POINT('Ctrl Pts',(-0.8252634783701,-1.35917443559929,1.91020759537532));
#17656=CARTESIAN_POINT('Ctrl Pts',(-0.798259149220139,-1.37485345097089,
1.91020766105751));
#17657=CARTESIAN_POINT('Ctrl Pts',(-0.769963363482765,-1.39128230047366,
1.91020772988089));
#17658=CARTESIAN_POINT('Ctrl Pts',(-0.741437699220515,-1.40728426915793,
1.9096825319157));
#17659=CARTESIAN_POINT('Ctrl Pts',(-0.712641620935351,-1.42280782457595,
1.90869858745619));
#17660=CARTESIAN_POINT('',(-0.719647344681869,-1.71930883511106,1.63615580822897));
#17661=CARTESIAN_POINT('Ctrl Pts',(-0.712641620935352,-1.42280782457595,
1.90869858745619));
#17662=CARTESIAN_POINT('Ctrl Pts',(-0.738348283935276,-1.4625344132382,
1.8616660525816));
#17663=CARTESIAN_POINT('Ctrl Pts',(-0.746832708799745,-1.5002914909622,
1.82419649029873));
#17664=CARTESIAN_POINT('Ctrl Pts',(-0.748805201903997,-1.58415905565693,
1.74786428230083));
#17665=CARTESIAN_POINT('Ctrl Pts',(-0.743412735108965,-1.64452676332901,
1.69596272615631));
#17666=CARTESIAN_POINT('Ctrl Pts',(-0.719647344681869,-1.71930883511106,
1.63615580822897));
#17667=CARTESIAN_POINT('',(-0.602229799711922,-1.76386916735271,1.63615580822897));
#17668=CARTESIAN_POINT('Origin',(0.,0.,1.63615580822897));
#17669=CARTESIAN_POINT('',(-0.425598593400272,-1.53333167412,1.90869858745619));
#17670=CARTESIAN_POINT('Ctrl Pts',(-0.602229799711921,-1.76386916735271,
1.63615580822897));
#17671=CARTESIAN_POINT('Ctrl Pts',(-0.56486102358392,-1.73560853660211,
1.67497485013891));
#17672=CARTESIAN_POINT('Ctrl Pts',(-0.533433211787428,-1.70762188310109,
1.71107791524129));
#17673=CARTESIAN_POINT('Ctrl Pts',(-0.492494397097019,-1.664207079411,1.7644774074943));
#17674=CARTESIAN_POINT('Ctrl Pts',(-0.470909637234242,-1.63987512035428,
1.79387050689047));
#17675=CARTESIAN_POINT('Ctrl Pts',(-0.442833202224615,-1.5926459267614,
1.84694613619249));
#17676=CARTESIAN_POINT('Ctrl Pts',(-0.431662037695392,-1.56765174845206,
1.87400707649573));
#17677=CARTESIAN_POINT('Ctrl Pts',(-0.425598593400271,-1.53333167412,1.90869858745619));
#17678=CARTESIAN_POINT('',(-0.238090659850088,-1.57338902476662,1.90869858745619));
#17679=CARTESIAN_POINT('Ctrl Pts',(-0.425598593400272,-1.53333167412,1.90869858745619));
#17680=CARTESIAN_POINT('Ctrl Pts',(-0.395279868504098,-1.5406776482735,
1.90972905962805));
#17681=CARTESIAN_POINT('Ctrl Pts',(-0.364864209844148,-1.54767214341183,
1.91020759537532));
#17682=CARTESIAN_POINT('Ctrl Pts',(-0.334336484432989,-1.55423897652106,
1.91020766105751));
#17683=CARTESIAN_POINT('Ctrl Pts',(-0.302348799329381,-1.56111986223385,
1.91020772988089));
#17684=CARTESIAN_POINT('Ctrl Pts',(-0.270274400184222,-1.56752372379171,
1.9096825319157));
#17685=CARTESIAN_POINT('Ctrl Pts',(-0.238090659850088,-1.57338902476662,
1.90869858745619));
#17686=CARTESIAN_POINT('',(-0.153129647965883,-1.85754313061971,1.63615580822897));
#17687=CARTESIAN_POINT('Ctrl Pts',(-0.238090659850089,-1.57338902476662,
1.90869858745619));
#17688=CARTESIAN_POINT('Ctrl Pts',(-0.25026295818307,-1.61911505151921,
1.86166605258207));
#17689=CARTESIAN_POINT('Ctrl Pts',(-0.246664547063089,-1.6576459977954,
1.82419649029927));
#17690=CARTESIAN_POINT('Ctrl Pts',(-0.226553376416707,-1.72488162993613,
1.76034062848752));
#17691=CARTESIAN_POINT('Ctrl Pts',(-0.206497613058332,-1.78308197878352,
1.70598062725551));
#17692=CARTESIAN_POINT('Ctrl Pts',(-0.153129647965884,-1.85754313061971,
1.63615580822897));
#17693=CARTESIAN_POINT('',(-0.0276890267571698,-1.86363850813291,1.63615580822897));
#17694=CARTESIAN_POINT('Origin',(0.,0.,1.63615580822897));
#17695=CARTESIAN_POINT('',(0.0690572297370874,-1.58980227845634,1.90869858745619));
#17696=CARTESIAN_POINT('Ctrl Pts',(-0.0276890267571705,-1.86363850813291,
1.63615580822897));
#17697=CARTESIAN_POINT('Ctrl Pts',(-0.000882223887656915,-1.82521346421937,
1.67497485013994));
#17698=CARTESIAN_POINT('Ctrl Pts',(0.0203590497666264,-1.78888484709669,
1.71107791524241));
#17699=CARTESIAN_POINT('Ctrl Pts',(0.0458782640980426,-1.73494412567807,
1.76447740749204));
#17700=CARTESIAN_POINT('Ctrl Pts',(0.0588876017641393,-1.70513299984438,
1.79387050688965));
#17701=CARTESIAN_POINT('Ctrl Pts',(0.0709952547834971,-1.65153927195932,
1.84694613619142));
#17702=CARTESIAN_POINT('Ctrl Pts',(0.0738960377459689,-1.62431631612213,
1.87400707649481));
#17703=CARTESIAN_POINT('Ctrl Pts',(0.0690572297370878,-1.58980227845634,
1.90869858745619));
#17704=CARTESIAN_POINT('',(0.259766273896473,-1.5699559447672,1.90869858745619));
#17705=CARTESIAN_POINT('Ctrl Pts',(0.0690572297370876,-1.58980227845634,
1.90869858745619));
#17706=CARTESIAN_POINT('Ctrl Pts',(0.100162081469028,-1.58741971380287,
1.90972905962805));
#17707=CARTESIAN_POINT('Ctrl Pts',(0.131250509699797,-1.58467291856134,
1.91020759537532));
#17708=CARTESIAN_POINT('Ctrl Pts',(0.162313364909724,-1.58148476202963,
1.91020766105751));
#17709=CARTESIAN_POINT('Ctrl Pts',(0.194861771890304,-1.57814413491694,
1.91020772988089));
#17710=CARTESIAN_POINT('Ctrl Pts',(0.227345240254553,-1.57432303476077,
1.90968253191571));
#17711=CARTESIAN_POINT('Ctrl Pts',(0.259766273896472,-1.5699559447672,1.90869858745619));
#17712=CARTESIAN_POINT('',(0.428377445609996,-1.81394816223928,1.63615580822897));
#17713=CARTESIAN_POINT('Ctrl Pts',(0.259766273896472,-1.5699559447672,1.90869858745619));
#17714=CARTESIAN_POINT('Ctrl Pts',(0.262319849600408,-1.61720542752026,
1.86166605258184));
#17715=CARTESIAN_POINT('Ctrl Pts',(0.277648859153229,-1.65273856486642,
1.824196490299));
#17716=CARTESIAN_POINT('Ctrl Pts',(0.325349196385585,-1.72174825234076,
1.74786428229831));
#17717=CARTESIAN_POINT('Ctrl Pts',(0.365195041949575,-1.76741714130283,
1.69596272615402));
#17718=CARTESIAN_POINT('Ctrl Pts',(0.428377445609996,-1.81394816223928,
1.63615580822897));
#17719=CARTESIAN_POINT('',(0.549562141057364,-1.78098192700405,1.63615580822897));
#17720=CARTESIAN_POINT('Origin',(0.,0.,1.63615580822897));
#17721=CARTESIAN_POINT('',(0.556953250077769,-1.49065195897357,1.90869858745619));
#17722=CARTESIAN_POINT('Ctrl Pts',(0.549562141057365,-1.78098192700405,
1.63615580822897));
#17723=CARTESIAN_POINT('Ctrl Pts',(0.563182934028143,-1.73615378095104,
1.6749748501387));
#17724=CARTESIAN_POINT('Ctrl Pts',(0.572158425678644,-1.69503929836728,
1.71107791524103));
#17725=CARTESIAN_POINT('Ctrl Pts',(0.579760041152732,-1.63585275285171,
1.76447740749537));
#17726=CARTESIAN_POINT('Ctrl Pts',(0.582920512008082,-1.60348058094729,
1.79387050689112));
#17727=CARTESIAN_POINT('Ctrl Pts',(0.577874201600642,-1.54876844626293,
1.84694613619459));
#17728=CARTESIAN_POINT('Ctrl Pts',(0.572220654147706,-1.52198148548948,
1.87400707649761));
#17729=CARTESIAN_POINT('Ctrl Pts',(0.556953250077769,-1.49065195897357,
1.90869858745619));
#17730=CARTESIAN_POINT('',(0.732195474855992,-1.41284463836769,1.90869858745619));
#17731=CARTESIAN_POINT('Ctrl Pts',(0.556953250077769,-1.49065195897357,
1.90869858745619));
#17732=CARTESIAN_POINT('Ctrl Pts',(0.585799469037704,-1.47877407754171,
1.90972905962805));
#17733=CARTESIAN_POINT('Ctrl Pts',(0.614517514878248,-1.46655486737661,
1.91020759537532));
#17734=CARTESIAN_POINT('Ctrl Pts',(0.643074851191361,-1.45392380017848,
1.91020766105751));
#17735=CARTESIAN_POINT('Ctrl Pts',(0.672997915195573,-1.44068866409761,
1.91020772988089));
#17736=CARTESIAN_POINT('Ctrl Pts',(0.702710744569794,-1.42701663813388,
1.90968253191571));
#17737=CARTESIAN_POINT('Ctrl Pts',(0.732195474855992,-1.41284463836769,
1.90869858745619));
#17738=CARTESIAN_POINT('',(0.967951970128402,-1.59279130921887,1.63615580822897));
#17739=CARTESIAN_POINT('Ctrl Pts',(0.732195474855992,-1.41284463836769,
1.90869858745619));
#17740=CARTESIAN_POINT('Ctrl Pts',(0.749224962814994,-1.4569924685421,1.8616660525824));
#17741=CARTESIAN_POINT('Ctrl Pts',(0.774784060541701,-1.48604956590099,
1.82419649029954));
#17742=CARTESIAN_POINT('Ctrl Pts',(0.841474943298512,-1.53694146401599,
1.74786428230295));
#17743=CARTESIAN_POINT('Ctrl Pts',(0.893483057171948,-1.56806211502227,
1.69596272615805));
#17744=CARTESIAN_POINT('Ctrl Pts',(0.967951970128402,-1.59279130921887,
1.63615580822897));
#17745=CARTESIAN_POINT('',(1.07301833748062,-1.52399042602929,1.63615580822897));
#17746=CARTESIAN_POINT('Origin',(0.,0.,1.63615580822897));
#17747=CARTESIAN_POINT('',(0.990330805779365,-1.24558623976355,1.90869858745619));
#17748=CARTESIAN_POINT('Ctrl Pts',(1.07301833748062,-1.52399042602929,1.63615580822897));
#17749=CARTESIAN_POINT('Ctrl Pts',(1.07211982243578,-1.4771472691025,1.6749748501427));
#17750=CARTESIAN_POINT('Ctrl Pts',(1.06795094842305,-1.43527149307552,1.71107791524426));
#17751=CARTESIAN_POINT('Ctrl Pts',(1.05689086595362,-1.37663271493145,1.76447740748792));
#17752=CARTESIAN_POINT('Ctrl Pts',(1.04989310109149,-1.34486831068513,1.79387050688826));
#17753=CARTESIAN_POINT('Ctrl Pts',(1.0281867952793,-1.29439337414807,1.8469461361916));
#17754=CARTESIAN_POINT('Ctrl Pts',(1.01453232602804,-1.27066450279334,1.87400707649487));
#17755=CARTESIAN_POINT('Ctrl Pts',(0.990330805779366,-1.24558623976355,
1.90869858745619));
#17756=CARTESIAN_POINT('',(1.13295228123076,-1.11743425489732,1.90869858745619));
#17757=CARTESIAN_POINT('Ctrl Pts',(0.990330805779366,-1.24558623976355,
1.90869858745619));
#17758=CARTESIAN_POINT('Ctrl Pts',(1.01409472307207,-1.22537573134593,1.90972905962805));
#17759=CARTESIAN_POINT('Ctrl Pts',(1.03763126410513,-1.20488020768447,1.91020759537532));
#17760=CARTESIAN_POINT('Ctrl Pts',(1.06088769047244,-1.18404264668309,1.91020766105751));
#17761=CARTESIAN_POINT('Ctrl Pts',(1.08525633350931,-1.16220854896825,1.91020772988089));
#17762=CARTESIAN_POINT('Ctrl Pts',(1.1092900251329,-1.14002391035689,1.90968253191571));
#17763=CARTESIAN_POINT('Ctrl Pts',(1.13295228123076,-1.11743425489732,1.90869858745619));
#17764=CARTESIAN_POINT('',(1.4127766116927,-1.21572094522251,1.63615580822897));
#17765=CARTESIAN_POINT('Ctrl Pts',(1.13295228123076,-1.11743425489733,1.90869858745619));
#17766=CARTESIAN_POINT('Ctrl Pts',(1.16279071651073,-1.15415893527858,1.86166605258442));
#17767=CARTESIAN_POINT('Ctrl Pts',(1.19607799984447,-1.17389568150877,1.82419649030168));
#17768=CARTESIAN_POINT('Ctrl Pts',(1.27523125986793,-1.20168813669816,1.74786428229881));
#17769=CARTESIAN_POINT('Ctrl Pts',(1.33431072550509,-1.2152142435953,1.69596272615425));
#17770=CARTESIAN_POINT('Ctrl Pts',(1.4127766116927,-1.21572094522251,1.63615580822897));
#17771=CARTESIAN_POINT('',(1.4914400228729,-1.11782012388912,1.63615580822897));
#17772=CARTESIAN_POINT('Origin',(0.,0.,1.63615580822897));
#17773=CARTESIAN_POINT('',(1.32676788217082,-0.878593860895847,1.90869858745619));
#17774=CARTESIAN_POINT('Ctrl Pts',(1.4914400228729,-1.11782012388912,1.63615580822897));
#17775=CARTESIAN_POINT('Ctrl Pts',(1.47611015272491,-1.07354729067132,1.67497485014032));
#17776=CARTESIAN_POINT('Ctrl Pts',(1.45920499148449,-1.03500931392226,1.71107791524254));
#17777=CARTESIAN_POINT('Ctrl Pts',(1.43056584900227,-0.9826582752975,1.76447740749182));
#17778=CARTESIAN_POINT('Ctrl Pts',(1.41409483840349,-0.954610959920599,
1.79387050688963));
#17779=CARTESIAN_POINT('Ctrl Pts',(1.37785330163609,-0.913314059998434,
1.84694613619306));
#17780=CARTESIAN_POINT('Ctrl Pts',(1.35753450517206,-0.894966025320543,
1.87400707649614));
#17781=CARTESIAN_POINT('Ctrl Pts',(1.32676788217082,-0.878593860895848,
1.90869858745619));
#17782=CARTESIAN_POINT('',(1.42280782457595,-0.712641620935351,1.90869858745619));
#17783=CARTESIAN_POINT('Ctrl Pts',(1.32676788217082,-0.878593860895847,
1.90869858745619));
#17784=CARTESIAN_POINT('Ctrl Pts',(1.34312331999875,-0.852029070871249,
1.90972905962805));
#17785=CARTESIAN_POINT('Ctrl Pts',(1.35917443559929,-0.825263478370106,
1.91020759537532));
#17786=CARTESIAN_POINT('Ctrl Pts',(1.37485345097089,-0.798259149220139,
1.91020766105751));
#17787=CARTESIAN_POINT('Ctrl Pts',(1.39128230047366,-0.769963363482759,
1.91020772988089));
#17788=CARTESIAN_POINT('Ctrl Pts',(1.40728426915793,-0.741437699220503,
1.9096825319157));
#17789=CARTESIAN_POINT('Ctrl Pts',(1.42280782457595,-0.712641620935351,
1.90869858745619));
#17790=CARTESIAN_POINT('',(1.71930883511106,-0.719647344681869,1.63615580822897));
#17791=CARTESIAN_POINT('Ctrl Pts',(1.42280782457595,-0.712641620935352,
1.90869858745619));
#17792=CARTESIAN_POINT('Ctrl Pts',(1.46253441323553,-0.738348283933551,
1.86166605258476));
#17793=CARTESIAN_POINT('Ctrl Pts',(1.50029149095869,-0.746832708799665,
1.82419649030192));
#17794=CARTESIAN_POINT('Ctrl Pts',(1.5841590556494,-0.748805201903815,1.74786428230768));
#17795=CARTESIAN_POINT('Ctrl Pts',(1.64452676332205,-0.743412735111191,
1.69596272616187));
#17796=CARTESIAN_POINT('Ctrl Pts',(1.71930883511106,-0.719647344681869,
1.63615580822897));
#17797=CARTESIAN_POINT('',(1.76386916735271,-0.602229799711922,1.63615580822897));
#17798=CARTESIAN_POINT('Origin',(0.,0.,1.63615580822897));
#17799=CARTESIAN_POINT('',(1.53333167412,-0.425598593400271,1.90869858745619));
#17800=CARTESIAN_POINT('Ctrl Pts',(1.76386916735271,-0.602229799711921,
1.63615580822897));
#17801=CARTESIAN_POINT('Ctrl Pts',(1.73560853660213,-0.564861023583931,
1.6749748501389));
#17802=CARTESIAN_POINT('Ctrl Pts',(1.7076218831011,-0.533433211787444,1.71107791524128));
#17803=CARTESIAN_POINT('Ctrl Pts',(1.66420707941097,-0.492494397096992,
1.76447740749434));
#17804=CARTESIAN_POINT('Ctrl Pts',(1.6398751203543,-0.470909637234254,1.79387050689044));
#17805=CARTESIAN_POINT('Ctrl Pts',(1.59264592676154,-0.442833202224699,
1.84694613619233));
#17806=CARTESIAN_POINT('Ctrl Pts',(1.56765174845221,-0.431662037695425,
1.87400707649557));
#17807=CARTESIAN_POINT('Ctrl Pts',(1.53333167412,-0.425598593400271,1.90869858745619));
#17808=CARTESIAN_POINT('',(1.57338902476662,-0.238090659850088,1.90869858745619));
#17809=CARTESIAN_POINT('Ctrl Pts',(1.53333167412,-0.425598593400272,1.90869858745619));
#17810=CARTESIAN_POINT('Ctrl Pts',(1.54067764827351,-0.395279868504085,
1.90972905962805));
#17811=CARTESIAN_POINT('Ctrl Pts',(1.54767214341184,-0.364864209844123,
1.91020759537532));
#17812=CARTESIAN_POINT('Ctrl Pts',(1.55423897652106,-0.334336484432989,
1.91020766105751));
#17813=CARTESIAN_POINT('Ctrl Pts',(1.56111986223385,-0.302348799329382,
1.91020772988089));
#17814=CARTESIAN_POINT('Ctrl Pts',(1.56752372379171,-0.270274400184223,
1.9096825319157));
#17815=CARTESIAN_POINT('Ctrl Pts',(1.57338902476662,-0.238090659850088,
1.90869858745619));
#17816=CARTESIAN_POINT('',(1.85754313061971,-0.153129647965884,1.63615580822897));
#17817=CARTESIAN_POINT('Ctrl Pts',(1.57338902476662,-0.238090659850088,
1.90869858745619));
#17818=CARTESIAN_POINT('Ctrl Pts',(1.61911505151656,-0.250262958182363,
1.8616660525848));
#17819=CARTESIAN_POINT('Ctrl Pts',(1.65764599779255,-0.246664547063935,
1.82419649030197));
#17820=CARTESIAN_POINT('Ctrl Pts',(1.72488162993741,-0.226553376416327,
1.7603406284863));
#17821=CARTESIAN_POINT('Ctrl Pts',(1.78308197878428,-0.206497613057801,
1.70598062725479));
#17822=CARTESIAN_POINT('Ctrl Pts',(1.85754313061971,-0.153129647965883,
1.63615580822897));
#17823=CARTESIAN_POINT('',(1.86363850813291,-0.0276890267571702,1.63615580822897));
#17824=CARTESIAN_POINT('Origin',(0.,0.,1.63615580822897));
#17825=CARTESIAN_POINT('',(1.58980227845634,0.0690572297370882,1.90869858745619));
#17826=CARTESIAN_POINT('Ctrl Pts',(1.86363850813291,-0.0276890267571701,
1.63615580822897));
#17827=CARTESIAN_POINT('Ctrl Pts',(1.82521346421932,-0.0008822238876082,
1.67497485014));
#17828=CARTESIAN_POINT('Ctrl Pts',(1.788884847097,0.0203590497664785,1.7110779152421));
#17829=CARTESIAN_POINT('Ctrl Pts',(1.73494412567664,0.045878264098721,1.76447740749345));
#17830=CARTESIAN_POINT('Ctrl Pts',(1.70513299984346,0.0588876017643422,
1.79387050689057));
#17831=CARTESIAN_POINT('Ctrl Pts',(1.6515392719567,0.0709952547840949,1.84694613619402));
#17832=CARTESIAN_POINT('Ctrl Pts',(1.62431631611976,0.0738960377456204,
1.87400707649719));
#17833=CARTESIAN_POINT('Ctrl Pts',(1.58980227845634,0.0690572297370886,
1.90869858745619));
#17834=CARTESIAN_POINT('',(1.5699559447672,0.259766273896473,1.90869858745619));
#17835=CARTESIAN_POINT('Ctrl Pts',(1.58980227845634,0.0690572297370888,
1.90869858745619));
#17836=CARTESIAN_POINT('Ctrl Pts',(1.58741971380287,0.100162081469027,1.90972905962805));
#17837=CARTESIAN_POINT('Ctrl Pts',(1.58467291856134,0.131250509699795,1.91020759537532));
#17838=CARTESIAN_POINT('Ctrl Pts',(1.58148476202963,0.162313364909724,1.91020766105751));
#17839=CARTESIAN_POINT('Ctrl Pts',(1.57814413491694,0.194861771890306,1.91020772988089));
#17840=CARTESIAN_POINT('Ctrl Pts',(1.57432303476077,0.227345240254558,1.9096825319157));
#17841=CARTESIAN_POINT('Ctrl Pts',(1.5699559447672,0.259766273896474,1.90869858745619));
#17842=CARTESIAN_POINT('',(1.81394816223928,0.428377445609997,1.63615580822897));
#17843=CARTESIAN_POINT('Ctrl Pts',(1.5699559447672,0.259766273896473,1.90869858745619));
#17844=CARTESIAN_POINT('Ctrl Pts',(1.61720542751669,0.262319849600217,1.86166605258539));
#17845=CARTESIAN_POINT('Ctrl Pts',(1.65273856486316,0.277648859150948,1.82419649030262));
#17846=CARTESIAN_POINT('Ctrl Pts',(1.72174825233291,0.325349196380191,1.74786428230698));
#17847=CARTESIAN_POINT('Ctrl Pts',(1.76741714129725,0.365195041941967,1.69596272616121));
#17848=CARTESIAN_POINT('Ctrl Pts',(1.81394816223928,0.428377445609997,1.63615580822897));
#17849=CARTESIAN_POINT('',(1.78098192700405,0.549562141057365,1.63615580822897));
#17850=CARTESIAN_POINT('Origin',(0.,0.,1.63615580822897));
#17851=CARTESIAN_POINT('',(1.49065195897357,0.556953250077769,1.90869858745619));
#17852=CARTESIAN_POINT('Ctrl Pts',(1.78098192700405,0.549562141057366,1.63615580822897));
#17853=CARTESIAN_POINT('Ctrl Pts',(1.73615378094971,0.563182934028546,1.67497485013986));
#17854=CARTESIAN_POINT('Ctrl Pts',(1.69503929836622,0.572158425678773,1.71107791524199));
#17855=CARTESIAN_POINT('Ctrl Pts',(1.63585275285416,0.579760041152422,1.76447740749316));
#17856=CARTESIAN_POINT('Ctrl Pts',(1.6034805809482,0.582920512008171,1.79387050689023));
#17857=CARTESIAN_POINT('Ctrl Pts',(1.54876844626462,0.577874201600796,1.84694613619294));
#17858=CARTESIAN_POINT('Ctrl Pts',(1.52198148549077,0.572220654148339,1.87400707649618));
#17859=CARTESIAN_POINT('Ctrl Pts',(1.49065195897357,0.556953250077769,1.90869858745619));
#17860=CARTESIAN_POINT('',(1.41284463836769,0.732195474855992,1.90869858745619));
#17861=CARTESIAN_POINT('Ctrl Pts',(1.49065195897357,0.55695325007777,1.90869858745619));
#17862=CARTESIAN_POINT('Ctrl Pts',(1.47877407754171,0.585799469037693,1.90972905962805));
#17863=CARTESIAN_POINT('Ctrl Pts',(1.46655486737662,0.614517514878226,1.91020759537532));
#17864=CARTESIAN_POINT('Ctrl Pts',(1.45392380017848,0.643074851191361,1.91020766105751));
#17865=CARTESIAN_POINT('Ctrl Pts',(1.44068866409761,0.672997915195586,1.91020772988089));
#17866=CARTESIAN_POINT('Ctrl Pts',(1.42701663813387,0.702710744569819,1.9096825319157));
#17867=CARTESIAN_POINT('Ctrl Pts',(1.41284463836769,0.732195474855992,1.90869858745619));
#17868=CARTESIAN_POINT('',(1.59279130921887,0.967951970128402,1.63615580822897));
#17869=CARTESIAN_POINT('Ctrl Pts',(1.41284463836769,0.732195474855992,1.90869858745619));
#17870=CARTESIAN_POINT('Ctrl Pts',(1.45699246854266,0.749224962815207,1.86166605258181));
#17871=CARTESIAN_POINT('Ctrl Pts',(1.48604956590136,0.774784060542144,1.82419649029901));
#17872=CARTESIAN_POINT('Ctrl Pts',(1.53694146401919,0.841474943302744,1.74786428229814));
#17873=CARTESIAN_POINT('Ctrl Pts',(1.56806211502394,0.89348305717702,1.69596272615399));
#17874=CARTESIAN_POINT('Ctrl Pts',(1.59279130921887,0.967951970128403,1.63615580822897));
#17875=CARTESIAN_POINT('',(1.5239904260293,1.07301833748062,1.63615580822897));
#17876=CARTESIAN_POINT('Origin',(0.,0.,1.63615580822897));
#17877=CARTESIAN_POINT('',(1.24558623976356,0.990330805779365,1.90869858745619));
#17878=CARTESIAN_POINT('Ctrl Pts',(1.5239904260293,1.07301833748062,1.63615580822897));
#17879=CARTESIAN_POINT('Ctrl Pts',(1.4771472691066,1.07211982243586,1.67497485013931));
#17880=CARTESIAN_POINT('Ctrl Pts',(1.43527149307835,1.06795094842359,1.71107791524167));
#17881=CARTESIAN_POINT('Ctrl Pts',(1.37663271492478,1.05689086595236,1.764477407494));
#17882=CARTESIAN_POINT('Ctrl Pts',(1.34486831068293,1.04989310109054,1.79387050689058));
#17883=CARTESIAN_POINT('Ctrl Pts',(1.29439337414837,1.02818679527943,1.84694613619127));
#17884=CARTESIAN_POINT('Ctrl Pts',(1.27066450279333,1.01453232602804,1.87400707649488));
#17885=CARTESIAN_POINT('Ctrl Pts',(1.24558623976356,0.990330805779365,1.90869858745619));
#17886=CARTESIAN_POINT('',(1.11743425489732,1.13295228123076,1.90869858745619));
#17887=CARTESIAN_POINT('Ctrl Pts',(1.24558623976356,0.990330805779365,1.90869858745619));
#17888=CARTESIAN_POINT('Ctrl Pts',(1.22537573134592,1.01409472307208,1.90972905962805));
#17889=CARTESIAN_POINT('Ctrl Pts',(1.20488020768446,1.03763126410514,1.91020759537532));
#17890=CARTESIAN_POINT('Ctrl Pts',(1.18404264668309,1.06088769047244,1.91020766105751));
#17891=CARTESIAN_POINT('Ctrl Pts',(1.16220854896825,1.08525633350931,1.91020772988089));
#17892=CARTESIAN_POINT('Ctrl Pts',(1.14002391035688,1.10929002513291,1.90968253191571));
#17893=CARTESIAN_POINT('Ctrl Pts',(1.11743425489733,1.13295228123076,1.90869858745619));
#17894=CARTESIAN_POINT('',(1.21572094522251,1.4127766116927,1.63615580822897));
#17895=CARTESIAN_POINT('Ctrl Pts',(1.11743425489733,1.13295228123076,1.90869858745619));
#17896=CARTESIAN_POINT('Ctrl Pts',(1.15415893527859,1.16279071651074,1.8616660525844));
#17897=CARTESIAN_POINT('Ctrl Pts',(1.17389568150877,1.19607799984457,1.82419649030161));
#17898=CARTESIAN_POINT('Ctrl Pts',(1.20168813669685,1.2752312598641,1.74786428230248));
#17899=CARTESIAN_POINT('Ctrl Pts',(1.21521424359528,1.33431072550103,1.69596272615734));
#17900=CARTESIAN_POINT('Ctrl Pts',(1.21572094522251,1.4127766116927,1.63615580822897));
#17901=CARTESIAN_POINT('',(1.11782012388912,1.4914400228729,1.63615580822897));
#17902=CARTESIAN_POINT('Origin',(0.,0.,1.63615580822897));
#17903=CARTESIAN_POINT('',(0.878593860895847,1.32676788217082,1.90869858745619));
#17904=CARTESIAN_POINT('Ctrl Pts',(1.11782012388912,1.4914400228729,1.63615580822897));
#17905=CARTESIAN_POINT('Ctrl Pts',(1.073547290672,1.47611015272516,1.67497485013972));
#17906=CARTESIAN_POINT('Ctrl Pts',(1.03500931392244,1.45920499148459,1.71107791524236));
#17907=CARTESIAN_POINT('Ctrl Pts',(0.982658275295369,1.4305658490011,1.76447740749399));
#17908=CARTESIAN_POINT('Ctrl Pts',(0.954610959919495,1.41409483840251,1.79387050689106));
#17909=CARTESIAN_POINT('Ctrl Pts',(0.913314059996841,1.3778533016347,1.8469461361951));
#17910=CARTESIAN_POINT('Ctrl Pts',(0.894966025319547,1.35753450517017,1.87400707649826));
#17911=CARTESIAN_POINT('Ctrl Pts',(0.878593860895847,1.32676788217082,1.90869858745619));
#17912=CARTESIAN_POINT('',(0.712641620935351,1.42280782457595,1.90869858745619));
#17913=CARTESIAN_POINT('Ctrl Pts',(0.878593860895847,1.32676788217082,1.90869858745619));
#17914=CARTESIAN_POINT('Ctrl Pts',(0.852029070871252,1.34312331999875,1.90972905962805));
#17915=CARTESIAN_POINT('Ctrl Pts',(0.825263478370114,1.35917443559928,1.91020759537532));
#17916=CARTESIAN_POINT('Ctrl Pts',(0.798259149220138,1.37485345097089,1.91020766105751));
#17917=CARTESIAN_POINT('Ctrl Pts',(0.769963363482762,1.39128230047366,1.91020772988089));
#17918=CARTESIAN_POINT('Ctrl Pts',(0.741437699220509,1.40728426915793,1.9096825319157));
#17919=CARTESIAN_POINT('Ctrl Pts',(0.71264162093535,1.42280782457595,1.90869858745619));
#17920=CARTESIAN_POINT('',(0.719647344681868,1.71930883511106,1.63615580822897));
#17921=CARTESIAN_POINT('Ctrl Pts',(0.712641620935351,1.42280782457595,1.90869858745619));
#17922=CARTESIAN_POINT('Ctrl Pts',(0.73834828393456,1.46253441323709,1.86166605258291));
#17923=CARTESIAN_POINT('Ctrl Pts',(0.746832708799669,1.50029149096089,1.82419649029994));
#17924=CARTESIAN_POINT('Ctrl Pts',(0.748805201904025,1.58415905565637,1.74786428230132));
#17925=CARTESIAN_POINT('Ctrl Pts',(0.743412735108989,1.64452676332897,1.69596272615633));
#17926=CARTESIAN_POINT('Ctrl Pts',(0.719647344681868,1.71930883511106,1.63615580822897));
#17927=CARTESIAN_POINT('',(0.602229799711921,1.76386916735271,1.63615580822897));
#17928=CARTESIAN_POINT('Origin',(0.,0.,1.63615580822897));
#17929=CARTESIAN_POINT('',(0.425598593400272,1.53333167412,1.90869858745619));
#17930=CARTESIAN_POINT('Ctrl Pts',(0.602229799711921,1.76386916735271,1.63615580822897));
#17931=CARTESIAN_POINT('Ctrl Pts',(0.564861023582366,1.73560853660092,1.67497485014054));
#17932=CARTESIAN_POINT('Ctrl Pts',(0.533433211786253,1.70762188309983,1.71107791524284));
#17933=CARTESIAN_POINT('Ctrl Pts',(0.492494397099151,1.66420707941326,1.76447740749151));
#17934=CARTESIAN_POINT('Ctrl Pts',(0.47090963723466,1.63987512035499,1.79387050688967));
#17935=CARTESIAN_POINT('Ctrl Pts',(0.442833202224378,1.592645926761,1.84694613619294));
#17936=CARTESIAN_POINT('Ctrl Pts',(0.431662037695335,1.56765174845163,1.87400707649615));
#17937=CARTESIAN_POINT('Ctrl Pts',(0.425598593400271,1.53333167412,1.90869858745619));
#17938=CARTESIAN_POINT('',(0.238090659850088,1.57338902476662,1.90869858745619));
#17939=CARTESIAN_POINT('Ctrl Pts',(0.425598593400271,1.53333167412,1.90869858745619));
#17940=CARTESIAN_POINT('Ctrl Pts',(0.3952798685041,1.5406776482735,1.90972905962805));
#17941=CARTESIAN_POINT('Ctrl Pts',(0.364864209844155,1.54767214341183,1.91020759537532));
#17942=CARTESIAN_POINT('Ctrl Pts',(0.334336484432989,1.55423897652106,1.91020766105751));
#17943=CARTESIAN_POINT('Ctrl Pts',(0.302348799329389,1.56111986223385,1.91020772988089));
#17944=CARTESIAN_POINT('Ctrl Pts',(0.270274400184237,1.56752372379171,1.90968253191571));
#17945=CARTESIAN_POINT('Ctrl Pts',(0.238090659850088,1.57338902476662,1.90869858745619));
#17946=CARTESIAN_POINT('',(0.153129647965883,1.85754313061971,1.63615580822897));
#17947=CARTESIAN_POINT('Ctrl Pts',(0.238090659850088,1.57338902476662,1.90869858745619));
#17948=CARTESIAN_POINT('Ctrl Pts',(0.250262958182808,1.61911505151823,1.86166605258308));
#17949=CARTESIAN_POINT('Ctrl Pts',(0.246664547063409,1.65764599779437,1.82419649030024));
#17950=CARTESIAN_POINT('Ctrl Pts',(0.226553376414497,1.72488162994349,1.76034062848052));
#17951=CARTESIAN_POINT('Ctrl Pts',(0.206497613055206,1.78308197878789,1.7059806272514));
#17952=CARTESIAN_POINT('Ctrl Pts',(0.153129647965883,1.85754313061971,1.63615580822897));
#17953=CARTESIAN_POINT('',(0.0276890267571704,1.86363850813291,1.63615580822897));
#17954=CARTESIAN_POINT('Origin',(0.,0.,1.63615580822897));
#17955=CARTESIAN_POINT('',(-0.0690572297370879,1.58980227845634,1.90869858745619));
#17956=CARTESIAN_POINT('Ctrl Pts',(0.0276890267571701,1.86363850813291,
1.63615580822897));
#17957=CARTESIAN_POINT('Ctrl Pts',(0.000882223887733506,1.82521346421949,
1.67497485013983));
#17958=CARTESIAN_POINT('Ctrl Pts',(-0.0203590497665907,1.78888484709677,
1.71107791524233));
#17959=CARTESIAN_POINT('Ctrl Pts',(-0.045878264098098,1.73494412567795,
1.76447740749215));
#17960=CARTESIAN_POINT('Ctrl Pts',(-0.0588876017641423,1.70513299984437,
1.79387050688967));
#17961=CARTESIAN_POINT('Ctrl Pts',(-0.0709952547835986,1.65153927195887,
1.84694613619187));
#17962=CARTESIAN_POINT('Ctrl Pts',(-0.0738960377459196,1.62431631612179,
1.87400707649515));
#17963=CARTESIAN_POINT('Ctrl Pts',(-0.0690572297370876,1.58980227845634,
1.90869858745619));
#17964=CARTESIAN_POINT('',(-0.259766273896473,1.5699559447672,1.90869858745619));
#17965=CARTESIAN_POINT('Ctrl Pts',(-0.0690572297370876,1.58980227845634,
1.90869858745619));
#17966=CARTESIAN_POINT('Ctrl Pts',(-0.100162081469031,1.58741971380287,
1.90972905962805));
#17967=CARTESIAN_POINT('Ctrl Pts',(-0.131250509699804,1.58467291856134,
1.91020759537532));
#17968=CARTESIAN_POINT('Ctrl Pts',(-0.162313364909724,1.58148476202963,
1.91020766105751));
#17969=CARTESIAN_POINT('Ctrl Pts',(-0.194861771890307,1.57814413491694,
1.91020772988089));
#17970=CARTESIAN_POINT('Ctrl Pts',(-0.22734524025456,1.57432303476077,1.9096825319157));
#17971=CARTESIAN_POINT('Ctrl Pts',(-0.259766273896473,1.5699559447672,1.90869858745619));
#17972=CARTESIAN_POINT('',(-0.428377445609996,1.81394816223928,1.63615580822897));
#17973=CARTESIAN_POINT('Ctrl Pts',(-0.259766273896472,1.5699559447672,1.90869858745619));
#17974=CARTESIAN_POINT('Ctrl Pts',(-0.262319849600359,1.61720542751929,
1.8616660525828));
#17975=CARTESIAN_POINT('Ctrl Pts',(-0.277648859152491,1.65273856486546,
1.82419649030008));
#17976=CARTESIAN_POINT('Ctrl Pts',(-0.325349196384362,1.72174825233888,
1.74786428230037));
#17977=CARTESIAN_POINT('Ctrl Pts',(-0.36519504194757,1.76741714130135,1.69596272615592));
#17978=CARTESIAN_POINT('Ctrl Pts',(-0.428377445609996,1.81394816223928,
1.63615580822897));
#17979=CARTESIAN_POINT('',(-0.549562141057365,1.78098192700405,1.63615580822897));
#17980=CARTESIAN_POINT('Origin',(0.,0.,1.63615580822897));
#17981=CARTESIAN_POINT('',(-0.55695325007777,1.49065195897357,1.90869858745619));
#17982=CARTESIAN_POINT('Ctrl Pts',(-0.549562141057366,1.78098192700405,
1.63615580822897));
#17983=CARTESIAN_POINT('Ctrl Pts',(-0.56318293402824,1.73615378095071,1.67497485013899));
#17984=CARTESIAN_POINT('Ctrl Pts',(-0.572158425678774,1.69503929836625,
1.71107791524196));
#17985=CARTESIAN_POINT('Ctrl Pts',(-0.579760041152499,1.63585275285353,
1.76447740749373));
#17986=CARTESIAN_POINT('Ctrl Pts',(-0.582920512008146,1.60348058094794,
1.79387050689049));
#17987=CARTESIAN_POINT('Ctrl Pts',(-0.577874201600643,1.54876844626296,
1.84694613619456));
#17988=CARTESIAN_POINT('Ctrl Pts',(-0.572220654147739,1.52198148548955,
1.87400707649754));
#17989=CARTESIAN_POINT('Ctrl Pts',(-0.55695325007777,1.49065195897357,1.90869858745619));
#17990=CARTESIAN_POINT('',(-0.732195474855993,1.41284463836769,1.90869858745619));
#17991=CARTESIAN_POINT('Ctrl Pts',(-0.55695325007777,1.49065195897357,1.90869858745619));
#17992=CARTESIAN_POINT('Ctrl Pts',(-0.585799469037708,1.47877407754171,
1.90972905962805));
#17993=CARTESIAN_POINT('Ctrl Pts',(-0.614517514878255,1.46655486737661,
1.91020759537532));
#17994=CARTESIAN_POINT('Ctrl Pts',(-0.643074851191362,1.45392380017848,
1.91020766105751));
#17995=CARTESIAN_POINT('Ctrl Pts',(-0.672997915195577,1.44068866409761,
1.91020772988089));
#17996=CARTESIAN_POINT('Ctrl Pts',(-0.702710744569799,1.42701663813388,
1.90968253191571));
#17997=CARTESIAN_POINT('Ctrl Pts',(-0.732195474855993,1.41284463836769,
1.90869858745619));
#17998=CARTESIAN_POINT('',(-0.967951970128403,1.59279130921887,1.63615580822897));
#17999=CARTESIAN_POINT('Ctrl Pts',(-0.732195474855993,1.41284463836769,
1.90869858745619));
#18000=CARTESIAN_POINT('Ctrl Pts',(-0.749224962815114,1.45699246854241,
1.86166605258207));
#18001=CARTESIAN_POINT('Ctrl Pts',(-0.774784060541914,1.48604956590117,
1.82419649029929));
#18002=CARTESIAN_POINT('Ctrl Pts',(-0.841474943298866,1.53694146401625,
1.74786428230256));
#18003=CARTESIAN_POINT('Ctrl Pts',(-0.893483057172211,1.56806211502235,
1.69596272615784));
#18004=CARTESIAN_POINT('Ctrl Pts',(-0.967951970128403,1.59279130921887,
1.63615580822897));
#18005=CARTESIAN_POINT('',(-1.07301833748062,1.5239904260293,1.63615580822897));
#18006=CARTESIAN_POINT('Origin',(0.,0.,1.63615580822897));
#18007=CARTESIAN_POINT('',(-0.990330805779365,1.24558623976355,1.90869858745619));
#18008=CARTESIAN_POINT('Ctrl Pts',(-1.07301833748062,1.5239904260293,1.63615580822897));
#18009=CARTESIAN_POINT('Ctrl Pts',(-1.07211982243592,1.47714726910886,1.67497485013742));
#18010=CARTESIAN_POINT('Ctrl Pts',(-1.06795094842396,1.43527149308025,1.71107791523994));
#18011=CARTESIAN_POINT('Ctrl Pts',(-1.05689086595159,1.37663271492071,1.7644774074977));
#18012=CARTESIAN_POINT('Ctrl Pts',(-1.04989310109001,1.34486831068169,1.79387050689188));
#18013=CARTESIAN_POINT('Ctrl Pts',(-1.02818679527844,1.29439337414607,1.8469461361937));
#18014=CARTESIAN_POINT('Ctrl Pts',(-1.01453232602662,1.27066450279187,1.87400707649691));
#18015=CARTESIAN_POINT('Ctrl Pts',(-0.990330805779365,1.24558623976356,
1.90869858745619));
#18016=CARTESIAN_POINT('',(-1.13295228123076,1.11743425489732,1.90869858745619));
#18017=CARTESIAN_POINT('Ctrl Pts',(-0.990330805779366,1.24558623976356,
1.90869858745619));
#18018=CARTESIAN_POINT('Ctrl Pts',(-1.01409472307207,1.22537573134593,1.90972905962805));
#18019=CARTESIAN_POINT('Ctrl Pts',(-1.03763126410513,1.20488020768446,1.91020759537532));
#18020=CARTESIAN_POINT('Ctrl Pts',(-1.06088769047244,1.18404264668309,1.91020766105751));
#18021=CARTESIAN_POINT('Ctrl Pts',(-1.08525633350932,1.16220854896824,1.91020772988089));
#18022=CARTESIAN_POINT('Ctrl Pts',(-1.10929002513292,1.14002391035687,1.9096825319157));
#18023=CARTESIAN_POINT('Ctrl Pts',(-1.13295228123076,1.11743425489732,1.90869858745619));
#18024=CARTESIAN_POINT('',(-1.4127766116927,1.21572094522251,1.63615580822897));
#18025=CARTESIAN_POINT('Ctrl Pts',(-1.13295228123076,1.11743425489733,1.90869858745619));
#18026=CARTESIAN_POINT('Ctrl Pts',(-1.16279071651051,1.15415893527831,1.86166605258477));
#18027=CARTESIAN_POINT('Ctrl Pts',(-1.19607799984402,1.17389568150863,1.82419649030211));
#18028=CARTESIAN_POINT('Ctrl Pts',(-1.27523125986877,1.20168813669844,1.74786428229801));
#18029=CARTESIAN_POINT('Ctrl Pts',(-1.33431072550602,1.21521424359531,1.69596272615354));
#18030=CARTESIAN_POINT('Ctrl Pts',(-1.4127766116927,1.21572094522251,1.63615580822897));
#18031=CARTESIAN_POINT('',(-1.4914400228729,1.11782012388913,1.63615580822897));
#18032=CARTESIAN_POINT('Origin',(0.,0.,1.63615580822897));
#18033=CARTESIAN_POINT('',(-1.32676788217082,0.878593860895847,1.90869858745619));
#18034=CARTESIAN_POINT('Ctrl Pts',(-1.4914400228729,1.11782012388913,1.63615580822897));
#18035=CARTESIAN_POINT('Ctrl Pts',(-1.4761101527255,1.07354729067302,1.67497485013884));
#18036=CARTESIAN_POINT('Ctrl Pts',(-1.45920499148537,1.03500931392384,1.71107791524092));
#18037=CARTESIAN_POINT('Ctrl Pts',(-1.43056584900109,0.982658275295367,
1.764477407494));
#18038=CARTESIAN_POINT('Ctrl Pts',(-1.41409483840328,0.954610959920349,
1.79387050688994));
#18039=CARTESIAN_POINT('Ctrl Pts',(-1.37785330163753,0.913314060000089,
1.84694613619094));
#18040=CARTESIAN_POINT('Ctrl Pts',(-1.35753450517376,0.894966025321443,
1.87400707649422));
#18041=CARTESIAN_POINT('Ctrl Pts',(-1.32676788217082,0.878593860895847,
1.90869858745619));
#18042=CARTESIAN_POINT('',(-1.42280782457595,0.712641620935351,1.90869858745619));
#18043=CARTESIAN_POINT('Ctrl Pts',(-1.32676788217082,0.878593860895847,
1.90869858745619));
#18044=CARTESIAN_POINT('Ctrl Pts',(-1.34312331999875,0.852029070871253,
1.90972905962805));
#18045=CARTESIAN_POINT('Ctrl Pts',(-1.35917443559928,0.825263478370115,
1.91020759537532));
#18046=CARTESIAN_POINT('Ctrl Pts',(-1.37485345097089,0.798259149220139,
1.91020766105751));
#18047=CARTESIAN_POINT('Ctrl Pts',(-1.39128230047365,0.769963363482771,
1.91020772988089));
#18048=CARTESIAN_POINT('Ctrl Pts',(-1.40728426915792,0.741437699220528,
1.90968253191571));
#18049=CARTESIAN_POINT('Ctrl Pts',(-1.42280782457595,0.712641620935352,
1.90869858745619));
#18050=CARTESIAN_POINT('',(-1.71930883511106,0.719647344681869,1.63615580822897));
#18051=CARTESIAN_POINT('Ctrl Pts',(-1.42280782457595,0.712641620935352,
1.90869858745619));
#18052=CARTESIAN_POINT('Ctrl Pts',(-1.46253441323564,0.738348283933626,
1.86166605258463));
#18053=CARTESIAN_POINT('Ctrl Pts',(-1.50029149095907,0.746832708799589,
1.82419649030161));
#18054=CARTESIAN_POINT('Ctrl Pts',(-1.58415905564638,0.748805201903826,
1.7478642823104));
#18055=CARTESIAN_POINT('Ctrl Pts',(-1.64452676331943,0.743412735112008,
1.69596272616397));
#18056=CARTESIAN_POINT('Ctrl Pts',(-1.71930883511106,0.719647344681869,
1.63615580822897));
#18057=CARTESIAN_POINT('',(-1.76386916735271,0.602229799711921,1.63615580822897));
#18058=CARTESIAN_POINT('Origin',(0.,0.,1.63615580822897));
#18059=CARTESIAN_POINT('',(-1.53333167412,0.425598593400271,1.90869858745619));
#18060=CARTESIAN_POINT('Ctrl Pts',(-1.76386916735271,0.602229799711921,
1.63615580822897));
#18061=CARTESIAN_POINT('Ctrl Pts',(-1.73560853660219,0.56486102358402,1.67497485013881));
#18062=CARTESIAN_POINT('Ctrl Pts',(-1.70762188310117,0.533433211787508,
1.71107791524119));
#18063=CARTESIAN_POINT('Ctrl Pts',(-1.66420707941108,0.492494397097101,
1.76447740749419));
#18064=CARTESIAN_POINT('Ctrl Pts',(-1.63987512035448,0.470909637234355,
1.79387050689024));
#18065=CARTESIAN_POINT('Ctrl Pts',(-1.59264592676207,0.442833202225016,
1.84694613619173));
#18066=CARTESIAN_POINT('Ctrl Pts',(-1.56765174845278,0.431662037695519,
1.874007076495));
#18067=CARTESIAN_POINT('Ctrl Pts',(-1.53333167412,0.425598593400271,1.90869858745619));
#18068=CARTESIAN_POINT('',(-1.57338902476662,0.238090659850088,1.90869858745619));
#18069=CARTESIAN_POINT('Ctrl Pts',(-1.53333167412,0.425598593400272,1.90869858745619));
#18070=CARTESIAN_POINT('Ctrl Pts',(-1.54067764827351,0.395279868504089,
1.90972905962805));
#18071=CARTESIAN_POINT('Ctrl Pts',(-1.54767214341184,0.364864209844131,
1.91020759537532));
#18072=CARTESIAN_POINT('Ctrl Pts',(-1.55423897652106,0.334336484432989,
1.91020766105751));
#18073=CARTESIAN_POINT('Ctrl Pts',(-1.56111986223385,0.302348799329394,
1.91020772988089));
#18074=CARTESIAN_POINT('Ctrl Pts',(-1.5675237237917,0.270274400184246,1.90968253191571));
#18075=CARTESIAN_POINT('Ctrl Pts',(-1.57338902476662,0.238090659850088,
1.90869858745619));
#18076=CARTESIAN_POINT('',(-1.85754313061971,0.153129647965883,1.63615580822897));
#18077=CARTESIAN_POINT('Ctrl Pts',(-1.57338902476662,0.238090659850089,
1.90869858745619));
#18078=CARTESIAN_POINT('Ctrl Pts',(-1.61911505151772,0.250262958182671,
1.86166605258361));
#18079=CARTESIAN_POINT('Ctrl Pts',(-1.6576459977938,0.246664547063569,1.82419649030078));
#18080=CARTESIAN_POINT('Ctrl Pts',(-1.72488162993957,0.226553376415675,
1.76034062848425));
#18081=CARTESIAN_POINT('Ctrl Pts',(-1.78308197878557,0.20649761305687,1.70598062725359));
#18082=CARTESIAN_POINT('Ctrl Pts',(-1.85754313061971,0.153129647965884,
1.63615580822897));
#18083=CARTESIAN_POINT('',(-1.86363850813291,0.0276890267571705,1.63615580822897));
#18084=CARTESIAN_POINT('Origin',(0.,0.,1.63615580822897));
#18085=CARTESIAN_POINT('Ctrl Pts',(-1.86363850813291,0.0276890267571706,
1.63615580822897));
#18086=CARTESIAN_POINT('Ctrl Pts',(-1.84930856933126,0.0176919049463911,
1.65063268159767));
#18087=CARTESIAN_POINT('Ctrl Pts',(-1.83526820787236,0.00847200864278421,
1.66473179212764));
#18088=CARTESIAN_POINT('Ctrl Pts',(-1.82153560215913,1.34132982498869E-12,
1.67846439784087));
#18089=CARTESIAN_POINT('Origin',(1.,0.,2.1));
#18090=CARTESIAN_POINT('',(-0.0502392594122347,0.998737211088938,2.10000000017302));
#18091=CARTESIAN_POINT('',(0.998737211088938,-0.0502392594122345,2.10000000017302));
#18092=CARTESIAN_POINT('Origin',(0.,0.,2.1));
#18093=CARTESIAN_POINT('',(0.0502392594122347,0.998737211088938,2.10000000017302));
#18094=CARTESIAN_POINT('Ctrl Pts',(-0.0501579420662037,0.998754980171774,
2.09996629646059));
#18095=CARTESIAN_POINT('Ctrl Pts',(-0.0455541516249309,0.998081971740583,
2.09994285225375));
#18096=CARTESIAN_POINT('Ctrl Pts',(-0.0409493960495382,0.997497248478843,
2.09992115702739));
#18097=CARTESIAN_POINT('Ctrl Pts',(-0.0363408599228962,0.997001962981805,
2.0999069394429));
#18098=CARTESIAN_POINT('Ctrl Pts',(-0.0344254769968775,0.996796114235378,
2.09990103038244));
#18099=CARTESIAN_POINT('Ctrl Pts',(-0.0325094393882293,0.996605701141417,
2.09989644467646));
#18100=CARTESIAN_POINT('Ctrl Pts',(-0.030591027199469,0.996431064903213,
2.0998929904383));
#18101=CARTESIAN_POINT('Ctrl Pts',(-0.0241570348712139,0.995845367927649,
2.09988140557563));
#18102=CARTESIAN_POINT('Ctrl Pts',(-0.0177195435991528,0.995439341015549,
2.09988208911745));
#18103=CARTESIAN_POINT('Ctrl Pts',(-0.0112042061332443,0.99522006377236,
2.09989207709953));
#18104=CARTESIAN_POINT('Ctrl Pts',(-0.0091395956891891,0.995150578179511,
2.09989524213775));
#18105=CARTESIAN_POINT('Ctrl Pts',(-0.00706875291999245,0.995099879623312,
2.09989939288935));
#18106=CARTESIAN_POINT('Ctrl Pts',(-0.00498909077113959,0.995068038205673,
2.09990458544879));
#18107=CARTESIAN_POINT('Ctrl Pts',(-0.00372411379059672,0.995048670319229,
2.09990774387919));
#18108=CARTESIAN_POINT('Ctrl Pts',(-0.00245612535390708,0.995036282497343,
2.09991128863539));
#18109=CARTESIAN_POINT('Ctrl Pts',(-0.00118453247084987,0.995030876493846,
2.09991524595687));
#18110=CARTESIAN_POINT('Ctrl Pts',(-4.37845315938809E-5,0.995026026759759,
2.09991879607608));
#18111=CARTESIAN_POINT('Ctrl Pts',(0.00109970303547405,0.995026788370882,
2.09992271042795));
#18112=CARTESIAN_POINT('Ctrl Pts',(0.00223928716687367,0.995033203141033,
2.09992682811702));
#18113=CARTESIAN_POINT('Ctrl Pts',(0.0036616886009847,0.995041209902455,
2.09993196771721));
#18114=CARTESIAN_POINT('Ctrl Pts',(0.00508052255109117,0.995058026539435,
2.09993740601942));
#18115=CARTESIAN_POINT('Ctrl Pts',(0.00649660255618722,0.99508373088496,
2.09994278957186));
#18116=CARTESIAN_POINT('Ctrl Pts',(0.00927146453168093,0.99513409951579,
2.09995333884513));
#18117=CARTESIAN_POINT('Ctrl Pts',(0.0120342525028786,0.995218575771198,
2.09996364717532));
#18118=CARTESIAN_POINT('Ctrl Pts',(0.0147909036437984,0.995337528356299,
2.0999713663429));
#18119=CARTESIAN_POINT('Ctrl Pts',(0.0158423647792016,0.995382900082279,
2.09997431064172));
#18120=CARTESIAN_POINT('Ctrl Pts',(0.0168924947237524,0.995433267490783,
2.09997688114622));
#18121=CARTESIAN_POINT('Ctrl Pts',(0.0179416114429507,0.995488633595717,
2.09997896362948));
#18122=CARTESIAN_POINT('Ctrl Pts',(0.0227736532195703,0.995743639856846,
2.09998855517054));
#18123=CARTESIAN_POINT('Ctrl Pts',(0.027584328345019,0.996104743818564,
2.09998770209067));
#18124=CARTESIAN_POINT('Ctrl Pts',(0.0323893668042188,0.996568206430001,
2.09998210436156));
#18125=CARTESIAN_POINT('Ctrl Pts',(0.0368950513274315,0.997002795316889,
2.09997685537102));
#18126=CARTESIAN_POINT('Ctrl Pts',(0.0413861399780065,0.997526459114176,
2.09996745668706));
#18127=CARTESIAN_POINT('Ctrl Pts',(0.0458741854723339,0.99813430097851,
2.09995967180744));
#18128=CARTESIAN_POINT('Ctrl Pts',(0.0473368418337277,0.998332396958311,
2.09995713471112));
#18129=CARTESIAN_POINT('Ctrl Pts',(0.0487991635875438,0.99853942952464,
2.09995477525694));
#18130=CARTESIAN_POINT('Ctrl Pts',(0.0502611215119263,0.998755291264538,
2.09995263618594));
#18131=CARTESIAN_POINT('',(0.998737211088938,0.0502392594122345,2.10000000017302));
#18132=CARTESIAN_POINT('Origin',(0.,0.,2.1));
#18133=CARTESIAN_POINT('Ctrl Pts',(0.998741489349531,0.0501276226578845,
2.09998790761528));
#18134=CARTESIAN_POINT('Ctrl Pts',(0.998209106442774,0.0465065804968853,
2.0999823604152));
#18135=CARTESIAN_POINT('Ctrl Pts',(0.997731917482903,0.0428858888083561,
2.09997532142456));
#18136=CARTESIAN_POINT('Ctrl Pts',(0.99731100353809,0.0392650986878338,
2.09996763820277));
#18137=CARTESIAN_POINT('Ctrl Pts',(0.996973673612343,0.0363633158470504,
2.0999614806956));
#18138=CARTESIAN_POINT('Ctrl Pts',(0.996672480569791,0.0334615115052595,
2.09995491761494));
#18139=CARTESIAN_POINT('Ctrl Pts',(0.996408345014525,0.0305539602702526,
2.09994817558028));
#18140=CARTESIAN_POINT('Ctrl Pts',(0.995823734577335,0.0241186857880212,
2.09993325345505));
#18141=CARTESIAN_POINT('Ctrl Pts',(0.995422878237189,0.0176782325627147,
2.09991691990568));
#18142=CARTESIAN_POINT('Ctrl Pts',(0.995209369745946,0.0111608079949593,
2.0999080411453));
#18143=CARTESIAN_POINT('Ctrl Pts',(0.99514171218205,0.00909553618039141,
2.09990522760241));
#18144=CARTESIAN_POINT('Ctrl Pts',(0.995092895768509,0.00702412914613266,
2.09990323613576));
#18145=CARTESIAN_POINT('Ctrl Pts',(0.99506286554661,0.00494410069252508,
2.0999025509242));
#18146=CARTESIAN_POINT('Ctrl Pts',(0.99504459933955,0.00367890090298719,
2.09990213413686));
#18147=CARTESIAN_POINT('Ctrl Pts',(0.995033286585864,0.00241076308799952,
2.09990220272711));
#18148=CARTESIAN_POINT('Ctrl Pts',(0.995028899524127,0.00113911783449072,
2.09990288388685));
#18149=CARTESIAN_POINT('Ctrl Pts',(0.995024963884268,-1.67708640180092E-6,
2.09990349495629));
#18150=CARTESIAN_POINT('Ctrl Pts',(0.995026593989671,-0.00114513314823198,
2.09990463268876));
#18151=CARTESIAN_POINT('Ctrl Pts',(0.995033805529301,-0.00228459200009584,
2.09990622411078));
#18152=CARTESIAN_POINT('Ctrl Pts',(0.995042806799174,-0.00370683706316931,
2.09990821048536));
#18153=CARTESIAN_POINT('Ctrl Pts',(0.995060508292759,-0.00512536873273449,
2.09991087886862));
#18154=CARTESIAN_POINT('Ctrl Pts',(0.99508694937675,-0.00654097371496716,
2.0999140064208));
#18155=CARTESIAN_POINT('Ctrl Pts',(0.995138761674284,-0.00931490486528927,
2.09992013497682));
#18156=CARTESIAN_POINT('Ctrl Pts',(0.995224111395307,-0.0120760964135134,
2.09992800145899));
#18157=CARTESIAN_POINT('Ctrl Pts',(0.995343089287915,-0.0148303143798948,
2.09993619328405));
#18158=CARTESIAN_POINT('Ctrl Pts',(0.995539967164857,-0.0193878382523947,
2.09994974865211));
#18159=CARTESIAN_POINT('Ctrl Pts',(0.995828617967945,-0.0239182715715797,
2.09996404004403));
#18160=CARTESIAN_POINT('Ctrl Pts',(0.996207735735797,-0.0284458173699921,
2.09997472302851));
#18161=CARTESIAN_POINT('Ctrl Pts',(0.99631850279087,-0.0297686330154764,
2.09997784428219));
#18162=CARTESIAN_POINT('Ctrl Pts',(0.996436986832906,-0.0310911807891784,
2.09998067371155));
#18163=CARTESIAN_POINT('Ctrl Pts',(0.996563166797704,-0.0324135784390754,
2.09998318511707));
#18164=CARTESIAN_POINT('Ctrl Pts',(0.997133221361869,-0.0383878931186965,
2.09999453111945));
#18165=CARTESIAN_POINT('Ctrl Pts',(0.997858925779834,-0.0443424598651534,
2.09999902027607));
#18166=CARTESIAN_POINT('Ctrl Pts',(0.998734041876947,-0.0502864563072932,
2.0999972397247));
#18167=CARTESIAN_POINT('Ctrl Pts',(0.999999999998244,-1.87406103457374E-6,
2.60499999999311));
#18168=CARTESIAN_POINT('Ctrl Pts',(1.00000006288704,0.033555619638003,2.60500024661583));
#18169=CARTESIAN_POINT('Ctrl Pts',(0.996432788538549,0.100793877077062,
2.59172126532562));
#18170=CARTESIAN_POINT('Ctrl Pts',(0.987779661769916,0.157562252712982,
2.55296011060328));
#18171=CARTESIAN_POINT('Ctrl Pts',(0.977968286593196,0.211192459212548,
2.49909481560466));
#18172=CARTESIAN_POINT('Ctrl Pts',(0.970281147530057,0.242238373929747,
2.44471009644067));
#18173=CARTESIAN_POINT('Ctrl Pts',(0.967388261055284,0.253317392831602,
2.37452193295668));
#18174=CARTESIAN_POINT('Ctrl Pts',(0.967116369990459,0.254356366300813,
2.34056467313598));
#18175=CARTESIAN_POINT('Ctrl Pts',(0.968060909182331,0.250746912814477,
2.30584393595531));
#18176=CARTESIAN_POINT('Ctrl Pts',(0.971275486994325,0.238235555290696,
2.25382796860057));
#18177=CARTESIAN_POINT('Ctrl Pts',(0.978160761261309,0.209370469448592,
2.20003517000389));
#18178=CARTESIAN_POINT('Ctrl Pts',(0.986928061083623,0.163194558725017,
2.1514224394046));
#18179=CARTESIAN_POINT('Ctrl Pts',(0.994800163464163,0.109016749833536,
2.11560611365411));
#18180=CARTESIAN_POINT('Ctrl Pts',(1.00003726905853,0.0393234864952561,
2.09484257852823));
#18181=CARTESIAN_POINT('Ctrl Pts',(1.00039359739908,-0.0285679116079913,
2.09347899005165));
#18182=CARTESIAN_POINT('Ctrl Pts',(0.995946129986918,-0.098499816085455,
2.11089539860567));
#18183=CARTESIAN_POINT('Ctrl Pts',(0.987595534630939,-0.160108842507484,
2.14787016428115));
#18184=CARTESIAN_POINT('Ctrl Pts',(0.978767296657426,-0.20640426202618,
2.19598850651528));
#18185=CARTESIAN_POINT('Ctrl Pts',(0.97062172581105,-0.241091125419321,
2.25963518301816));
#18186=CARTESIAN_POINT('Ctrl Pts',(0.967038345237899,-0.254607790735269,
2.32400532558939));
#18187=CARTESIAN_POINT('Ctrl Pts',(0.967372392238064,-0.253367892292085,
2.39214155711082));
#18188=CARTESIAN_POINT('Ctrl Pts',(0.971848592631414,-0.236216524025834,
2.45101723423612));
#18189=CARTESIAN_POINT('Ctrl Pts',(0.977999994055034,-0.208938409888944,
2.49656599568729));
#18190=CARTESIAN_POINT('Ctrl Pts',(0.982365078241419,-0.187417224408925,
2.52354132496555));
#18191=CARTESIAN_POINT('Ctrl Pts',(0.986694720178997,-0.163267539196543,
2.54663242388917));
#18192=CARTESIAN_POINT('Ctrl Pts',(0.99244571253526,-0.125541882265517,
2.57418619605903));
#18193=CARTESIAN_POINT('Ctrl Pts',(0.998300344088637,-0.0706101566680352,
2.59849422048893));
#18194=CARTESIAN_POINT('Ctrl Pts',(0.999999955756101,-0.0236095057558304,
2.60499982649452));
#18195=CARTESIAN_POINT('Ctrl Pts',(0.999999999998244,-1.87406103457374E-6,
2.60499999999311));
#18196=CARTESIAN_POINT('Ctrl Pts',(0.983333333331803,-1.72646341714646E-6,
2.58833333332708));
#18197=CARTESIAN_POINT('Ctrl Pts',(0.983325070408895,0.0309254949332375,
2.58831701644367));
#18198=CARTESIAN_POINT('Ctrl Pts',(0.980235431771385,0.0928701985922922,
2.5763334457126));
#18199=CARTESIAN_POINT('Ctrl Pts',(0.97262951086769,0.146010496479255,2.54070549738907));
#18200=CARTESIAN_POINT('Ctrl Pts',(0.963966193226361,0.196619990384259,
2.49071684326285));
#18201=CARTESIAN_POINT('Ctrl Pts',(0.957121635980358,0.226408216243534,
2.43967803502293));
#18202=CARTESIAN_POINT('Ctrl Pts',(0.954530758590317,0.237116103160976,
2.37322988185745));
#18203=CARTESIAN_POINT('Ctrl Pts',(0.954292056495262,0.238108034056394,
2.34106055897148));
#18204=CARTESIAN_POINT('Ctrl Pts',(0.955131698824161,0.234634460337268,
2.30818704053657));
#18205=CARTESIAN_POINT('Ctrl Pts',(0.958005717805603,0.222572733944937,
2.2590085409333));
#18206=CARTESIAN_POINT('Ctrl Pts',(0.964133168526514,0.194921019608955,
2.20849850875947));
#18207=CARTESIAN_POINT('Ctrl Pts',(0.971886775166395,0.151277899039362,
2.16333241887712));
#18208=CARTESIAN_POINT('Ctrl Pts',(0.978798486508062,0.100613721566294,
2.13040797264567));
#18209=CARTESIAN_POINT('Ctrl Pts',(0.983369400970407,0.0361963313628681,
2.11151394416968));
#18210=CARTESIAN_POINT('Ctrl Pts',(0.983676824334791,-0.0262950908417384,
2.11028422573118));
#18211=CARTESIAN_POINT('Ctrl Pts',(0.979801092832465,-0.0908603189323969,
2.12610656815928));
#18212=CARTESIAN_POINT('Ctrl Pts',(0.972473802924845,-0.148358154753562,
2.16004581981554));
#18213=CARTESIAN_POINT('Ctrl Pts',(0.964672149439096,-0.192110727398231,
2.20471275196644));
#18214=CARTESIAN_POINT('Ctrl Pts',(0.957427193110245,-0.225297504050057,
2.26446164543395));
#18215=CARTESIAN_POINT('Ctrl Pts',(0.954222830159563,-0.238355411074918,
2.32536038420973));
#18216=CARTESIAN_POINT('Ctrl Pts',(0.954522079095343,-0.2371523061421,2.3899277120541));
#18217=CARTESIAN_POINT('Ctrl Pts',(0.958517953243843,-0.220614507903057,
2.4455635357429));
#18218=CARTESIAN_POINT('Ctrl Pts',(0.963982071416956,-0.194581079725971,
2.48825477624319));
#18219=CARTESIAN_POINT('Ctrl Pts',(0.967849868185066,-0.174169675975904,
2.51340938027297));
#18220=CARTESIAN_POINT('Ctrl Pts',(0.97167321111088,-0.151401045973518,
2.53482806141593));
#18221=CARTESIAN_POINT('Ctrl Pts',(0.976733295652627,-0.116052309467583,
2.56023494607926));
#18222=CARTESIAN_POINT('Ctrl Pts',(0.981853837292877,-0.0650450913579237,
2.58243716495324));
#18223=CARTESIAN_POINT('Ctrl Pts',(0.983332905880957,-0.0217501188318965,
2.58833203941799));
#18224=CARTESIAN_POINT('Ctrl Pts',(0.983333333331803,-1.72646341714646E-6,
2.58833333332708));
#18225=CARTESIAN_POINT('Ctrl Pts',(0.966666666665363,-1.57886579971917E-6,
2.57166666666104));
#18226=CARTESIAN_POINT('Ctrl Pts',(0.966675031089233,0.0282574067618839,
2.57168340910161));
#18227=CARTESIAN_POINT('Ctrl Pts',(0.964030995123869,0.0849671350523733,
2.56092437077672));
#18228=CARTESIAN_POINT('Ctrl Pts',(0.957496079669552,0.134432741424285,
2.52848314020048));
#18229=CARTESIAN_POINT('Ctrl Pts',(0.949965488618089,0.18202293386404,2.48231761863255));
#18230=CARTESIAN_POINT('Ctrl Pts',(0.943960096058651,0.210589600813346,
2.4346289274524));
#18231=CARTESIAN_POINT('Ctrl Pts',(0.941686431722323,0.220882428486858,
2.3719223211333));
#18232=CARTESIAN_POINT('Ctrl Pts',(0.94146963989202,0.221854615130021,2.34155719007975));
#18233=CARTESIAN_POINT('Ctrl Pts',(0.942215861234142,0.218493014540143,
2.31051805593517));
#18234=CARTESIAN_POINT('Ctrl Pts',(0.944737453851974,0.206900615314252,
2.26419080172698));
#18235=CARTESIAN_POINT('Ctrl Pts',(0.950105713610565,0.180489574889026,
2.21697132240232));
#18236=CARTESIAN_POINT('Ctrl Pts',(0.956837948144641,0.139371349739201,
2.17526823220057));
#18237=CARTESIAN_POINT('Ctrl Pts',(0.962797300252717,0.0922406494407946,
2.14521214199563));
#18238=CARTESIAN_POINT('Ctrl Pts',(0.966692768725039,0.0330593334366949,
2.12821013824094));
#18239=CARTESIAN_POINT('Ctrl Pts',(0.966958180635997,-0.0240006511464648,
2.12709572724774));
#18240=CARTESIAN_POINT('Ctrl Pts',(0.963654605188848,-0.08321040561347,
2.1413234011611));
#18241=CARTESIAN_POINT('Ctrl Pts',(0.957353720921044,-0.136587098613656,
2.17220985324203));
#18242=CARTESIAN_POINT('Ctrl Pts',(0.950573235959199,-0.177820331414012,
2.21345060010943));
#18243=CARTESIAN_POINT('Ctrl Pts',(0.944223169736954,-0.209514123317684,
2.26930212368042));
#18244=CARTESIAN_POINT('Ctrl Pts',(0.941403959395846,-0.222103494504004,
2.32673583609555));
#18245=CARTESIAN_POINT('Ctrl Pts',(0.941667556372663,-0.220946133881027,
2.38772812706794));
#18246=CARTESIAN_POINT('Ctrl Pts',(0.945187704752525,-0.205008502652309,
2.44011245850097));
#18247=CARTESIAN_POINT('Ctrl Pts',(0.94997031235299,-0.180221173921234,
2.47994404421443));
#18248=CARTESIAN_POINT('Ctrl Pts',(0.953336718390379,-0.160920110206714,
2.5032802399603));
#18249=CARTESIAN_POINT('Ctrl Pts',(0.956651963018509,-0.139538170190601,
2.5230099883211));
#18250=CARTESIAN_POINT('Ctrl Pts',(0.961021973375283,-0.10656485199273,
2.54628159282629));
#18251=CARTESIAN_POINT('Ctrl Pts',(0.965409168116845,-0.0594989402485911,
2.56637680898634));
#18252=CARTESIAN_POINT('Ctrl Pts',(0.966667022710479,-0.0198905682807695,
2.57166766119149));
#18253=CARTESIAN_POINT('Ctrl Pts',(0.966666666665363,-1.57886579971917E-6,
2.57166666666104));
#18254=CARTESIAN_POINT('Ctrl Pts',(0.949999999998922,-1.43126818229188E-6,
2.554999999995));
#18255=CARTESIAN_POINT('Ctrl Pts',(0.950000038611092,0.0256272820571184,
2.55500017892945));
#18256=CARTESIAN_POINT('Ctrl Pts',(0.947833638356706,0.077043456567603,
2.5455365511637));
#18257=CARTESIAN_POINT('Ctrl Pts',(0.942345928767326,0.122880985190557,
2.51622852698627));
#18258=CARTESIAN_POINT('Ctrl Pts',(0.935963395251255,0.167450465035751,
2.47393964629074));
#18259=CARTESIAN_POINT('Ctrl Pts',(0.930800584508952,0.194759443127133,
2.42959686603466));
#18260=CARTESIAN_POINT('Ctrl Pts',(0.928828929257356,0.204681138816232,
2.37063027003408));
#18261=CARTESIAN_POINT('Ctrl Pts',(0.928645326396822,0.205606282885602,
2.34205307591525));
#18262=CARTESIAN_POINT('Ctrl Pts',(0.929286650875972,0.202380562062934,
2.31286116051643));
#18263=CARTESIAN_POINT('Ctrl Pts',(0.931467684663253,0.191237793968494,
2.26937137405972));
#18264=CARTESIAN_POINT('Ctrl Pts',(0.93607812087577,0.166040125049389,2.2254346611579));
#18265=CARTESIAN_POINT('Ctrl Pts',(0.941796662227414,0.127454690053546,
2.18717821167308));
#18266=CARTESIAN_POINT('Ctrl Pts',(0.946795623296616,0.0838376211735529,
2.16001400098719));
#18267=CARTESIAN_POINT('Ctrl Pts',(0.950024900636915,0.0299321783043069,
2.14488150388239));
#18268=CARTESIAN_POINT('Ctrl Pts',(0.950241407571709,-0.0217278303802119,
2.14390096292727));
#18269=CARTESIAN_POINT('Ctrl Pts',(0.947509568034395,-0.0755709084604119,
2.15653457071471));
#18270=CARTESIAN_POINT('Ctrl Pts',(0.942231989214949,-0.124836410859733,
2.18438550877642));
#18271=CARTESIAN_POINT('Ctrl Pts',(0.936478088740869,-0.163526796786063,
2.22217484556059));
#18272=CARTESIAN_POINT('Ctrl Pts',(0.931028637036149,-0.19372050194842,
2.27412858609622));
#18273=CARTESIAN_POINT('Ctrl Pts',(0.92858844431751,-0.205851114843653,
2.32809089471589));
#18274=CARTESIAN_POINT('Ctrl Pts',(0.928817243229942,-0.204730547731042,
2.38551428201123));
#18275=CARTESIAN_POINT('Ctrl Pts',(0.931857065364954,-0.189406486529532,
2.43465876000775));
#18276=CARTESIAN_POINT('Ctrl Pts',(0.935952389714912,-0.165863843758261,
2.47163282477033));
#18277=CARTESIAN_POINT('Ctrl Pts',(0.938821508334025,-0.147672561773693,
2.49314829526772));
#18278=CARTESIAN_POINT('Ctrl Pts',(0.941630453950392,-0.127671676967576,
2.51120562584786));
#18279=CARTESIAN_POINT('Ctrl Pts',(0.945309556492649,-0.0970752791947962,
2.53233034284651));
#18280=CARTESIAN_POINT('Ctrl Pts',(0.948962661321086,-0.0539338749384796,
2.55031975345065));
#18281=CARTESIAN_POINT('Ctrl Pts',(0.949999972835335,-0.0180311813568356,
2.55499987411497));
#18282=CARTESIAN_POINT('Ctrl Pts',(0.949999999998922,-1.43126818229188E-6,
2.554999999995));
#18283=CARTESIAN_POINT('',(0.987458837468112,0.157876674357314,2.54999999999916));
#18284=CARTESIAN_POINT('Ctrl Pts',(0.998741489263531,0.0501276243402692,
2.09998790795724));
#18285=CARTESIAN_POINT('Ctrl Pts',(0.997746174412029,0.0695985876399753,
2.10394554683626));
#18286=CARTESIAN_POINT('Ctrl Pts',(0.994363645806935,0.112020975270126,
2.11759217250489));
#18287=CARTESIAN_POINT('Ctrl Pts',(0.986928061083623,0.163194558725017,
2.1514224394046));
#18288=CARTESIAN_POINT('Ctrl Pts',(0.978160761261309,0.209370469448592,
2.20003517000389));
#18289=CARTESIAN_POINT('Ctrl Pts',(0.971275486994325,0.238235555290696,
2.25382796860057));
#18290=CARTESIAN_POINT('Ctrl Pts',(0.968060909182331,0.250746912814477,
2.30584393595531));
#18291=CARTESIAN_POINT('Ctrl Pts',(0.967116369990459,0.254356366300813,
2.34056467313598));
#18292=CARTESIAN_POINT('Ctrl Pts',(0.967388261055284,0.253317392831602,
2.37452193295668));
#18293=CARTESIAN_POINT('Ctrl Pts',(0.970281147530057,0.242238373929747,
2.44471009644067));
#18294=CARTESIAN_POINT('Ctrl Pts',(0.977968286593196,0.211192459212548,
2.49909481560466));
#18295=CARTESIAN_POINT('Ctrl Pts',(0.98494013308223,0.173083472433883,2.53737085347425));
#18296=CARTESIAN_POINT('Ctrl Pts',(0.986199840262143,0.165761961406214,
2.54388428246999));
#18297=CARTESIAN_POINT('Ctrl Pts',(0.987440095705288,0.157976027584706,
2.55002758371622));
#18298=CARTESIAN_POINT('',(0.972500000001548,-1.63052496584468E-6,2.57749999999709));
#18299=CARTESIAN_POINT('Ctrl Pts',(0.987458837468451,0.157876674355192,
2.55));
#18300=CARTESIAN_POINT('Ctrl Pts',(0.985294697406766,0.146794280964263,
2.55388665064189));
#18301=CARTESIAN_POINT('Ctrl Pts',(0.983354421647032,0.135549889588831,
2.55740912752908));
#18302=CARTESIAN_POINT('Ctrl Pts',(0.977055328631449,0.0935709003424381,
2.56892572544489));
#18303=CARTESIAN_POINT('Ctrl Pts',(0.974161715360584,0.0622013742464855,
2.57437596695135));
#18304=CARTESIAN_POINT('Ctrl Pts',(0.972834706545006,0.0246194032981655,
2.57687004873351));
#18305=CARTESIAN_POINT('Ctrl Pts',(0.972691422895011,0.0189840464089377,
2.57713968402705));
#18306=CARTESIAN_POINT('Ctrl Pts',(0.972559701868467,0.0105124985263587,
2.57738760007473));
#18307=CARTESIAN_POINT('Ctrl Pts',(0.972529696233088,0.0076814295447408,
2.5774440907214));
#18308=CARTESIAN_POINT('Ctrl Pts',(0.972504563213093,0.00323267114025078,
2.57749140831944));
#18309=CARTESIAN_POINT('Ctrl Pts',(0.972499996930093,0.00161553516506767,
2.57750000577993));
#18310=CARTESIAN_POINT('Ctrl Pts',(0.972500000001548,-1.63052496584468E-6,
2.57749999999708));
#18311=CARTESIAN_POINT('',(0.949999999998922,-1.43126818229188E-6,2.554999999995));
#18312=CARTESIAN_POINT('Ctrl Pts',(0.972500000001548,-1.63052496584468E-6,
2.57749999999709));
#18313=CARTESIAN_POINT('Ctrl Pts',(0.965000000000673,-1.56410603799375E-6,
2.56999999999639));
#18314=CARTESIAN_POINT('Ctrl Pts',(0.957499999999797,-1.49768711014282E-6,
2.5624999999957));
#18315=CARTESIAN_POINT('Ctrl Pts',(0.949999999998922,-1.43126818229188E-6,
2.554999999995));
#18316=CARTESIAN_POINT('',(0.950017413548361,2.77722566314428E-6,2.14493017758226));
#18317=CARTESIAN_POINT('Ctrl Pts',(0.949999999998922,-1.43126818229188E-6,
2.554999999995));
#18318=CARTESIAN_POINT('Ctrl Pts',(0.950000038611092,0.0256272820571184,
2.55500017892945));
#18319=CARTESIAN_POINT('Ctrl Pts',(0.947833638356706,0.077043456567603,
2.5455365511637));
#18320=CARTESIAN_POINT('Ctrl Pts',(0.942345928767326,0.122880985190557,
2.51622852698627));
#18321=CARTESIAN_POINT('Ctrl Pts',(0.935963395251255,0.167450465035751,
2.47393964629074));
#18322=CARTESIAN_POINT('Ctrl Pts',(0.930800584508952,0.194759443127133,
2.42959686603466));
#18323=CARTESIAN_POINT('Ctrl Pts',(0.928828929257356,0.204681138816232,
2.37063027003408));
#18324=CARTESIAN_POINT('Ctrl Pts',(0.928645326396822,0.205606282885602,
2.34205307591525));
#18325=CARTESIAN_POINT('Ctrl Pts',(0.929286650875972,0.202380562062934,
2.31286116051643));
#18326=CARTESIAN_POINT('Ctrl Pts',(0.931467684663253,0.191237793968494,
2.26937137405972));
#18327=CARTESIAN_POINT('Ctrl Pts',(0.93607812087577,0.166040125049389,2.2254346611579));
#18328=CARTESIAN_POINT('Ctrl Pts',(0.941796662227414,0.127454690053546,
2.18717821167308));
#18329=CARTESIAN_POINT('Ctrl Pts',(0.946795623296616,0.0838376211735529,
2.16001400098719));
#18330=CARTESIAN_POINT('Ctrl Pts',(0.949571221584807,0.0375053185605399,
2.14700745845955));
#18331=CARTESIAN_POINT('Ctrl Pts',(0.950019209030419,0.0100740119424525,
2.1449223021834));
#18332=CARTESIAN_POINT('Ctrl Pts',(0.950017413548361,2.77722566314337E-6,
2.14493017758226));
#18333=CARTESIAN_POINT('Ctrl Pts',(0.950017413548361,2.77722566314337E-6,
2.14493017758226));
#18334=CARTESIAN_POINT('Ctrl Pts',(0.950016105516441,-0.0073342476264757,
2.14493591491227));
#18335=CARTESIAN_POINT('Ctrl Pts',(0.949714588734556,-0.0321111444056223,
2.14633727826451));
#18336=CARTESIAN_POINT('Ctrl Pts',(0.947509568034395,-0.0755709084604119,
2.15653457071471));
#18337=CARTESIAN_POINT('Ctrl Pts',(0.942231989214949,-0.124836410859733,
2.18438550877642));
#18338=CARTESIAN_POINT('Ctrl Pts',(0.936478088740869,-0.163526796786063,
2.22217484556059));
#18339=CARTESIAN_POINT('Ctrl Pts',(0.931028637036149,-0.19372050194842,
2.27412858609622));
#18340=CARTESIAN_POINT('Ctrl Pts',(0.92858844431751,-0.205851114843653,
2.32809089471589));
#18341=CARTESIAN_POINT('Ctrl Pts',(0.928817243229942,-0.204730547731042,
2.38551428201123));
#18342=CARTESIAN_POINT('Ctrl Pts',(0.931857065364954,-0.189406486529532,
2.43465876000775));
#18343=CARTESIAN_POINT('Ctrl Pts',(0.935952389714912,-0.165863843758261,
2.47163282477033));
#18344=CARTESIAN_POINT('Ctrl Pts',(0.938821508334025,-0.147672561773693,
2.49314829526772));
#18345=CARTESIAN_POINT('Ctrl Pts',(0.941630453950392,-0.127671676967576,
2.51120562584786));
#18346=CARTESIAN_POINT('Ctrl Pts',(0.945309556492649,-0.0970752791947962,
2.53233034284651));
#18347=CARTESIAN_POINT('Ctrl Pts',(0.948962661321086,-0.0539338749384796,
2.55031975345065));
#18348=CARTESIAN_POINT('Ctrl Pts',(0.949999972835335,-0.0180311813568356,
2.55499987411497));
#18349=CARTESIAN_POINT('Ctrl Pts',(0.949999999998922,-1.43126818229188E-6,
2.554999999995));
#18350=CARTESIAN_POINT('',(0.987458837468112,-0.157876674357314,2.54999999999916));
#18351=CARTESIAN_POINT('Ctrl Pts',(0.972500000001548,-1.63052496584468E-6,
2.57749999999708));
#18352=CARTESIAN_POINT('Ctrl Pts',(0.972500001100936,-0.00058047386256792,
2.57749999792719));
#18353=CARTESIAN_POINT('Ctrl Pts',(0.972500587629742,-0.00115932100720252,
2.5774988936244));
#18354=CARTESIAN_POINT('Ctrl Pts',(0.972506627935273,-0.00414265020170195,
2.57748752117621));
#18355=CARTESIAN_POINT('Ctrl Pts',(0.972521597304209,-0.00654688441944551,
2.57745933671442));
#18356=CARTESIAN_POINT('Ctrl Pts',(0.972586968658232,-0.0128156465435284,
2.57733627628346));
#18357=CARTESIAN_POINT('Ctrl Pts',(0.972653363288269,-0.016678636176991,
2.57721129835072));
#18358=CARTESIAN_POINT('Ctrl Pts',(0.972929256482295,-0.0281987946478753,
2.57669227394828));
#18359=CARTESIAN_POINT('Ctrl Pts',(0.973215079278776,-0.0358422720486581,
2.57615478699383));
#18360=CARTESIAN_POINT('Ctrl Pts',(0.974562717145952,-0.0623401377173552,
2.57362665221117));
#18361=CARTESIAN_POINT('Ctrl Pts',(0.976141626745025,-0.0810078079633483,
2.57067014303824));
#18362=CARTESIAN_POINT('Ctrl Pts',(0.980686505593143,-0.119336271682647,
2.56227318576719));
#18363=CARTESIAN_POINT('Ctrl Pts',(0.98374047439577,-0.138835225480723,
2.55667793110024));
#18364=CARTESIAN_POINT('Ctrl Pts',(0.987458837468451,-0.157876674355193,
2.55));
#18365=CARTESIAN_POINT('Ctrl Pts',(0.987454582400007,-0.157881308716372,
2.55005328965836));
#18366=CARTESIAN_POINT('Ctrl Pts',(0.987200786017512,-0.159467384180762,
2.5487918471679));
#18367=CARTESIAN_POINT('Ctrl Pts',(0.985506430965119,-0.169895526191808,
2.54029497054242));
#18368=CARTESIAN_POINT('Ctrl Pts',(0.982365078241419,-0.187417224408925,
2.52354132496555));
#18369=CARTESIAN_POINT('Ctrl Pts',(0.977999994055034,-0.208938409888944,
2.49656599568729));
#18370=CARTESIAN_POINT('Ctrl Pts',(0.971848592631414,-0.236216524025834,
2.45101723423612));
#18371=CARTESIAN_POINT('Ctrl Pts',(0.967372392238064,-0.253367892292085,
2.39214155711082));
#18372=CARTESIAN_POINT('Ctrl Pts',(0.967038345237899,-0.254607790735269,
2.32400532558939));
#18373=CARTESIAN_POINT('Ctrl Pts',(0.97062172581105,-0.241091125419321,
2.25963518301816));
#18374=CARTESIAN_POINT('Ctrl Pts',(0.978767296657426,-0.20640426202618,
2.19598850651528));
#18375=CARTESIAN_POINT('Ctrl Pts',(0.987595534630939,-0.160108842507484,
2.14787016428115));
#18376=CARTESIAN_POINT('Ctrl Pts',(0.995084474394307,-0.104856939129847,
2.11471063719305));
#18377=CARTESIAN_POINT('Ctrl Pts',(0.997930949375477,-0.066177461549665,
2.10319104189167));
#18378=CARTESIAN_POINT('Ctrl Pts',(0.998734041791771,-0.0502864579926989,
2.09999724006344));
#18379=CARTESIAN_POINT('Origin',(0.,0.,2.325));
#18380=CARTESIAN_POINT('',(-1.,-1.22464679914735E-16,2.55));
#18381=CARTESIAN_POINT('Origin',(0.,0.,2.55));
#18382=CARTESIAN_POINT('',(-0.157876674357314,0.987458837468112,2.54999999999916));
#18383=CARTESIAN_POINT('Origin',(0.,0.,2.55));
#18384=CARTESIAN_POINT('Ctrl Pts',(-0.0501579437468834,0.998754980083996,
2.09996629680899));
#18385=CARTESIAN_POINT('Ctrl Pts',(-0.0826028085300709,0.997060472227549,
2.10669206239688));
#18386=CARTESIAN_POINT('Ctrl Pts',(-0.13333014615059,0.991871170579173,
2.12768221339602));
#18387=CARTESIAN_POINT('Ctrl Pts',(-0.184987608046235,0.98297944306662,
2.17252130019332));
#18388=CARTESIAN_POINT('Ctrl Pts',(-0.230530876255093,0.973454395083889,
2.2311541204646));
#18389=CARTESIAN_POINT('Ctrl Pts',(-0.255122284839583,0.966868905933786,
2.30756601931672));
#18390=CARTESIAN_POINT('Ctrl Pts',(-0.253875658998481,0.967246420818866,
2.38036927332879));
#18391=CARTESIAN_POINT('Ctrl Pts',(-0.237007380156922,0.971620587810882,
2.45580858562862));
#18392=CARTESIAN_POINT('Ctrl Pts',(-0.204967295321157,0.979117858283225,
2.50518732075992));
#18393=CARTESIAN_POINT('Ctrl Pts',(-0.173082478875929,0.984944804714717,
2.53735038518041));
#18394=CARTESIAN_POINT('Ctrl Pts',(-0.165770169783921,0.986201917446944,
2.54386940226406));
#18395=CARTESIAN_POINT('Ctrl Pts',(-0.157987843541269,0.987440871532657,
2.55001521460453));
#18396=CARTESIAN_POINT('Origin',(0.,0.,2.325));
#18397=CARTESIAN_POINT('',(0.157876674357314,0.987458837468112,2.54999999999916));
#18398=CARTESIAN_POINT('Ctrl Pts',(0.15787361447241,0.987459601094589,2.55002190145526));
#18399=CARTESIAN_POINT('Ctrl Pts',(0.159367603381274,0.987220783300611,
2.54883298459783));
#18400=CARTESIAN_POINT('Ctrl Pts',(0.16716148070395,0.985957317693993,2.54248953138653));
#18401=CARTESIAN_POINT('Ctrl Pts',(0.197782154055467,0.980628932028831,
2.51447081618292));
#18402=CARTESIAN_POINT('Ctrl Pts',(0.240862072091396,0.970821978192215,
2.45070211099161));
#18403=CARTESIAN_POINT('Ctrl Pts',(0.253753920072381,0.967257584978194,
2.38208598978509));
#18404=CARTESIAN_POINT('Ctrl Pts',(0.25377137321269,0.967257227319747,2.31770963275004));
#18405=CARTESIAN_POINT('Ctrl Pts',(0.247407872853293,0.96898626609141,2.28335835196792));
#18406=CARTESIAN_POINT('Ctrl Pts',(0.223542473616943,0.974765351154506,
2.22546113156583));
#18407=CARTESIAN_POINT('Ctrl Pts',(0.202625228604316,0.979486896662666,
2.19281789751093));
#18408=CARTESIAN_POINT('Ctrl Pts',(0.152664347670934,0.988739671565028,
2.14180432402534));
#18409=CARTESIAN_POINT('Ctrl Pts',(0.102949265500905,0.995581814195147,
2.11270476782457));
#18410=CARTESIAN_POINT('Ctrl Pts',(0.0581205001812461,0.998362457461274,
2.10152203482183));
#18411=CARTESIAN_POINT('Ctrl Pts',(0.0502611231985831,0.998755291180234,
2.09995263652274));
#18412=CARTESIAN_POINT('Origin',(0.,0.,2.55));
#18413=CARTESIAN_POINT('Origin',(0.705,0.,2.35));
#18414=CARTESIAN_POINT('',(0.501,-1.25526296912604E-17,2.145));
#18415=CARTESIAN_POINT('',(0.705,-2.51052593825207E-17,2.145));
#18416=CARTESIAN_POINT('',(0.457138928554548,-0.205,2.35));
#18417=CARTESIAN_POINT('Ctrl Pts',(0.457138928554548,-0.205,2.35));
#18418=CARTESIAN_POINT('Ctrl Pts',(0.457138928554548,-0.205,2.32390927987453));
#18419=CARTESIAN_POINT('Ctrl Pts',(0.459609069157102,-0.199722778787908,
2.29632432035936));
#18420=CARTESIAN_POINT('Ctrl Pts',(0.468177727272261,-0.178715671123715,
2.24592797085052));
#18421=CARTESIAN_POINT('Ctrl Pts',(0.474117890962221,-0.162998335554875,
2.22308455526839));
#18422=CARTESIAN_POINT('Ctrl Pts',(0.485018345626291,-0.126935588134045,
2.18702180784756));
#18423=CARTESIAN_POINT('Ctrl Pts',(0.490733376060334,-0.104084611878653,
2.17128923329376));
#18424=CARTESIAN_POINT('Ctrl Pts',(0.498772107838147,-0.0536585253249439,
2.1502704112139));
#18425=CARTESIAN_POINT('Ctrl Pts',(0.501,-0.0260615896504235,2.145));
#18426=CARTESIAN_POINT('Ctrl Pts',(0.501,-6.24500451351651E-17,2.145));
#18427=CARTESIAN_POINT('Ctrl Pts',(0.501,0.,2.145));
#18428=CARTESIAN_POINT('Ctrl Pts',(0.501,0.0260615896504235,2.145));
#18429=CARTESIAN_POINT('Ctrl Pts',(0.498772107838147,0.0536585253249438,
2.1502704112139));
#18430=CARTESIAN_POINT('Ctrl Pts',(0.490733376060334,0.104084611878653,
2.17128923329376));
#18431=CARTESIAN_POINT('Ctrl Pts',(0.485018345626291,0.126935588134045,
2.18702180784756));
#18432=CARTESIAN_POINT('Ctrl Pts',(0.474117890962221,0.162998335554875,
2.22308455526839));
#18433=CARTESIAN_POINT('Ctrl Pts',(0.468177727272261,0.178715671123715,
2.24592797085052));
#18434=CARTESIAN_POINT('Ctrl Pts',(0.459609069157102,0.199722778787908,
2.29632432035936));
#18435=CARTESIAN_POINT('Ctrl Pts',(0.457138928554548,0.205,2.32390927987453));
#18436=CARTESIAN_POINT('Ctrl Pts',(0.457138928554548,0.205,2.37609072012547));
#18437=CARTESIAN_POINT('Ctrl Pts',(0.459609069157102,0.199722778787908,
2.40367567964064));
#18438=CARTESIAN_POINT('Ctrl Pts',(0.468177727272261,0.178715671123715,
2.45407202914948));
#18439=CARTESIAN_POINT('Ctrl Pts',(0.474117890962221,0.162998335554875,
2.47691544473161));
#18440=CARTESIAN_POINT('Ctrl Pts',(0.485018345626291,0.126935588134045,
2.51297819215244));
#18441=CARTESIAN_POINT('Ctrl Pts',(0.490733376060334,0.104084611878653,
2.52871076670624));
#18442=CARTESIAN_POINT('Ctrl Pts',(0.498772107838147,0.0536585253249439,
2.5497295887861));
#18443=CARTESIAN_POINT('Ctrl Pts',(0.501,0.0260615896504235,2.555));
#18444=CARTESIAN_POINT('Ctrl Pts',(0.501,-0.0260615896504234,2.555));
#18445=CARTESIAN_POINT('Ctrl Pts',(0.498772107838147,-0.0536585253249438,
2.5497295887861));
#18446=CARTESIAN_POINT('Ctrl Pts',(0.490733376060334,-0.104084611878653,
2.52871076670624));
#18447=CARTESIAN_POINT('Ctrl Pts',(0.485018345626291,-0.126935588134045,
2.51297819215244));
#18448=CARTESIAN_POINT('Ctrl Pts',(0.474117890962222,-0.162998335554875,
2.47691544473161));
#18449=CARTESIAN_POINT('Ctrl Pts',(0.468177727272261,-0.178715671123715,
2.45407202914948));
#18450=CARTESIAN_POINT('Ctrl Pts',(0.459609069157102,-0.199722778787908,
2.40367567964064));
#18451=CARTESIAN_POINT('Ctrl Pts',(0.457138928554548,-0.205,2.37609072012547));
#18452=CARTESIAN_POINT('Ctrl Pts',(0.457138928554548,-0.205,2.35));
#18453=CARTESIAN_POINT('Ctrl Pts',(1.8740610339731E-6,0.999999999998244,
2.60499999999311));
#18454=CARTESIAN_POINT('Ctrl Pts',(-0.0335556196380034,1.00000006288704,
2.60500024661583));
#18455=CARTESIAN_POINT('Ctrl Pts',(-0.100756673071006,0.996441174833638,
2.59168345968582));
#18456=CARTESIAN_POINT('Ctrl Pts',(-0.157603488695687,0.98777358833807,
2.55296445525625));
#18457=CARTESIAN_POINT('Ctrl Pts',(-0.204967295321157,0.979117858283225,
2.50518732075992));
#18458=CARTESIAN_POINT('Ctrl Pts',(-0.237007380156922,0.971620587810882,
2.45580858562862));
#18459=CARTESIAN_POINT('Ctrl Pts',(-0.253875658998481,0.967246420818866,
2.38036927332879));
#18460=CARTESIAN_POINT('Ctrl Pts',(-0.255122284839583,0.966868905933786,
2.30756601931672));
#18461=CARTESIAN_POINT('Ctrl Pts',(-0.230530876255093,0.973454395083889,
2.2311541204646));
#18462=CARTESIAN_POINT('Ctrl Pts',(-0.184987608046235,0.98297944306662,
2.17252130019332));
#18463=CARTESIAN_POINT('Ctrl Pts',(-0.130000247114384,0.992444341497521,
2.12479183461179));
#18464=CARTESIAN_POINT('Ctrl Pts',(-0.0547900546441262,0.999800917250482,
2.09586490599377));
#18465=CARTESIAN_POINT('Ctrl Pts',(0.00901292386013043,1.00025490450459,
2.09401178448709));
#18466=CARTESIAN_POINT('Ctrl Pts',(0.0460479466138129,0.999088187246804,
2.09861314679373));
#18467=CARTESIAN_POINT('Ctrl Pts',(0.101662133244068,0.995758958476132,
2.11195137517568));
#18468=CARTESIAN_POINT('Ctrl Pts',(0.152664347670934,0.988739671565028,
2.14180432402534));
#18469=CARTESIAN_POINT('Ctrl Pts',(0.202625228604316,0.979486896662666,
2.19281789751093));
#18470=CARTESIAN_POINT('Ctrl Pts',(0.223542473616943,0.974765351154506,
2.22546113156583));
#18471=CARTESIAN_POINT('Ctrl Pts',(0.247407872853293,0.96898626609141,2.28335835196792));
#18472=CARTESIAN_POINT('Ctrl Pts',(0.25377137321269,0.967257227319747,2.31770963275004));
#18473=CARTESIAN_POINT('Ctrl Pts',(0.253753920072381,0.967257584978194,
2.38208598978509));
#18474=CARTESIAN_POINT('Ctrl Pts',(0.240862072091396,0.970821978192215,
2.45070211099161));
#18475=CARTESIAN_POINT('Ctrl Pts',(0.197782154055467,0.980628932028831,
2.51447081618292));
#18476=CARTESIAN_POINT('Ctrl Pts',(0.16267570908935,0.986737898868484,2.54659412947604));
#18477=CARTESIAN_POINT('Ctrl Pts',(0.136234199434897,0.990851168416345,
2.56664374352278));
#18478=CARTESIAN_POINT('Ctrl Pts',(0.0840473157184407,0.997329420352096,
2.59494454511583));
#18479=CARTESIAN_POINT('Ctrl Pts',(0.03365753814838,0.999999936925475,2.60499975264892));
#18480=CARTESIAN_POINT('Ctrl Pts',(1.8740610339731E-6,0.999999999998244,
2.60499999999311));
#18481=CARTESIAN_POINT('Ctrl Pts',(1.72646341657069E-6,0.983333333331803,
2.58833333332708));
#18482=CARTESIAN_POINT('Ctrl Pts',(-0.0309211194933883,0.983327802047045,
2.58831966882739));
#18483=CARTESIAN_POINT('Ctrl Pts',(-0.0928377960476621,0.98023976768212,
2.57629404074584));
#18484=CARTESIAN_POINT('Ctrl Pts',(-0.146048423576797,0.972626976944164,
2.54070953195264));
#18485=CARTESIAN_POINT('Ctrl Pts',(-0.190747496194426,0.964977664234015,
2.49636747507197));
#18486=CARTESIAN_POINT('Ctrl Pts',(-0.221374849129247,0.95831490086092,
2.45011538765543));
#18487=CARTESIAN_POINT('Ctrl Pts',(-0.237650481571607,0.954402200933291,
2.37878285196974));
#18488=CARTESIAN_POINT('Ctrl Pts',(-0.238858199349336,0.954071300725052,
2.30977107620483));
#18489=CARTESIAN_POINT('Ctrl Pts',(-0.215099921034606,0.959955138122488,
2.23759648199501));
#18490=CARTESIAN_POINT('Ctrl Pts',(-0.17183883952112,0.968399947196108,
2.18290355895676));
#18491=CARTESIAN_POINT('Ctrl Pts',(-0.120099054224975,0.976743248230922,
2.13876052168788));
#18492=CARTESIAN_POINT('Ctrl Pts',(-0.0504163434655785,0.983158893045571,
2.11245900795287));
#18493=CARTESIAN_POINT('Ctrl Pts',(0.00827833993718029,0.983561344274991,
2.1107555539468));
#18494=CARTESIAN_POINT('Ctrl Pts',(0.0424518621317906,0.982538668939213,
2.11495120932668));
#18495=CARTESIAN_POINT('Ctrl Pts',(0.0937720299455498,0.979640570051344,
2.12707976132422));
#18496=CARTESIAN_POINT('Ctrl Pts',(0.141360481904814,0.973477223378796,
2.15443787690997));
#18497=CARTESIAN_POINT('Ctrl Pts',(0.188538345234594,0.965310317630362,
2.20179163355866));
#18498=CARTESIAN_POINT('Ctrl Pts',(0.208490757001602,0.961105657569896,
2.23236164151278));
#18499=CARTESIAN_POINT('Ctrl Pts',(0.231400254955185,0.955964354544338,
2.28688145033855));
#18500=CARTESIAN_POINT('Ctrl Pts',(0.237544330067899,0.954413219989739,
2.31941255684048));
#18501=CARTESIAN_POINT('Ctrl Pts',(0.237537755869605,0.954418441564086,
2.38038851320367));
#18502=CARTESIAN_POINT('Ctrl Pts',(0.225032695661137,0.957606932779055,
2.44537253850971));
#18503=CARTESIAN_POINT('Ctrl Pts',(0.183910350012796,0.966318757498156,
2.50501316984723));
#18504=CARTESIAN_POINT('Ctrl Pts',(0.150857782836235,0.971711641804196,
2.53478061849988));
#18505=CARTESIAN_POINT('Ctrl Pts',(0.126062259734711,0.975331110231934,
2.55328561568025));
#18506=CARTESIAN_POINT('Ctrl Pts',(0.0774389729843563,0.981016367853088,
2.57924416260037));
#18507=CARTESIAN_POINT('Ctrl Pts',(0.0310095625324942,0.983324489370319,
2.58831441049439));
#18508=CARTESIAN_POINT('Ctrl Pts',(1.72646341657069E-6,0.983333333331803,
2.58833333332708));
#18509=CARTESIAN_POINT('Ctrl Pts',(1.57886579916828E-6,0.966666666665363,
2.57166666666104));
#18510=CARTESIAN_POINT('Ctrl Pts',(-0.028261782201734,0.966672299451083,
2.57168075671789));
#18511=CARTESIAN_POINT('Ctrl Pts',(-0.0849369725180309,0.964038061600584,
2.56088137505698));
#18512=CARTESIAN_POINT('Ctrl Pts',(-0.134467081311291,0.957489301980934,
2.52849464185));
#18513=CARTESIAN_POINT('Ctrl Pts',(-0.176493077367449,0.950850885491106,
2.48751717131812));
#18514=CARTESIAN_POINT('Ctrl Pts',(-0.205749279945383,0.945011607194673,
2.44443170330968));
#18515=CARTESIAN_POINT('Ctrl Pts',(-0.221405615759076,0.941576404880082,
2.37718285612148));
#18516=CARTESIAN_POINT('Ctrl Pts',(-0.222592256095046,0.941273043800734,
2.31198020634687));
#18517=CARTESIAN_POINT('Ctrl Pts',(-0.19967059846768,0.946452066132863,
2.24404982314633));
#18518=CARTESIAN_POINT('Ctrl Pts',(-0.158679713896286,0.953815819341673,
2.19329233666131));
#18519=CARTESIAN_POINT('Ctrl Pts',(-0.110198993644362,0.961036297799555,
2.15273846356872));
#18520=CARTESIAN_POINT('Ctrl Pts',(-0.046075343884759,0.966525769606431,
2.12903238312702));
#18521=CARTESIAN_POINT('Ctrl Pts',(0.00757919676247354,0.966850980745995,
2.12753983018364));
#18522=CARTESIAN_POINT('Ctrl Pts',(0.0388114474174279,0.965990205488828,
2.13128917659776));
#18523=CARTESIAN_POINT('Ctrl Pts',(0.0859427838572395,0.963505820548163,
2.14224095850635));
#18524=CARTESIAN_POINT('Ctrl Pts',(0.130095057847622,0.958228990545236,
2.16703937038342));
#18525=CARTESIAN_POINT('Ctrl Pts',(0.17448083867517,0.95111834103327,2.21079555546396));
#18526=CARTESIAN_POINT('Ctrl Pts',(0.193473476747956,0.947464227672504,
2.23924962741081));
#18527=CARTESIAN_POINT('Ctrl Pts',(0.215362766008526,0.942940862740997,
2.29040473546289));
#18528=CARTESIAN_POINT('Ctrl Pts',(0.221328116324425,0.941582271034106,
2.32111335094323));
#18529=CARTESIAN_POINT('Ctrl Pts',(0.221307475198179,0.941576462552143,
2.37869131092512));
#18530=CARTESIAN_POINT('Ctrl Pts',(0.209212867982546,0.944395419867102,
2.44004063866257));
#18531=CARTESIAN_POINT('Ctrl Pts',(0.170035598298793,0.952016482602868,
2.49557168347949));
#18532=CARTESIAN_POINT('Ctrl Pts',(0.139037988014577,0.956682144907831,
2.52295666497662));
#18533=CARTESIAN_POINT('Ctrl Pts',(0.115891644338605,0.959813980610051,
2.53993061096407));
#18534=CARTESIAN_POINT('Ctrl Pts',(0.0708540967431303,0.964686661475804,
2.56350215110508));
#18535=CARTESIAN_POINT('Ctrl Pts',(0.0283530954373026,0.96667540882895,
2.57168516269162));
#18536=CARTESIAN_POINT('Ctrl Pts',(1.57886579916828E-6,0.966666666665363,
2.57166666666104));
#18537=CARTESIAN_POINT('Ctrl Pts',(1.43126818176587E-6,0.949999999998922,
2.554999999995));
#18538=CARTESIAN_POINT('Ctrl Pts',(-0.0256272820571188,0.950000038611092,
2.55500017892945));
#18539=CARTESIAN_POINT('Ctrl Pts',(-0.0770180954946874,0.947836654449066,
2.545491956117));
#18540=CARTESIAN_POINT('Ctrl Pts',(-0.122912016192401,0.942342690587028,
2.51623971854639));
#18541=CARTESIAN_POINT('Ctrl Pts',(-0.162273278240718,0.936710691441896,
2.47869732563017));
#18542=CARTESIAN_POINT('Ctrl Pts',(-0.190116748917708,0.931705920244711,
2.43873850533649));
#18543=CARTESIAN_POINT('Ctrl Pts',(-0.205180438332203,0.928732184994508,
2.37559643476243));
#18544=CARTESIAN_POINT('Ctrl Pts',(-0.2063281706048,0.928475438592001,2.31418526323498));
#18545=CARTESIAN_POINT('Ctrl Pts',(-0.184239643247193,0.932952809171462,
2.25049218467674));
#18546=CARTESIAN_POINT('Ctrl Pts',(-0.14553094537117,0.939236323471161,
2.20367459542476));
#18547=CARTESIAN_POINT('Ctrl Pts',(-0.100297800754953,0.945335204532955,
2.16670715064481));
#18548=CARTESIAN_POINT('Ctrl Pts',(-0.0417016327062113,0.94988374540152,
2.14562648508612));
#18549=CARTESIAN_POINT('Ctrl Pts',(0.0068446128395234,0.950157420516395,
2.14428359964335));
#18550=CARTESIAN_POINT('Ctrl Pts',(0.0352153629354055,0.949440687181237,
2.14762723913071));
#18551=CARTESIAN_POINT('Ctrl Pts',(0.0780526805587212,0.947387432123376,
2.15736934465489));
#18552=CARTESIAN_POINT('Ctrl Pts',(0.118791192081503,0.942966542359005,
2.17967292326805));
#18553=CARTESIAN_POINT('Ctrl Pts',(0.160393955305448,0.936941762000965,
2.2197692915117));
#18554=CARTESIAN_POINT('Ctrl Pts',(0.178421760132616,0.933804534087895,
2.24615013735776));
#18555=CARTESIAN_POINT('Ctrl Pts',(0.199355148110418,0.929918951193924,
2.29392783383353));
#18556=CARTESIAN_POINT('Ctrl Pts',(0.205101073179634,0.928738263704097,
2.32281627503367));
#18557=CARTESIAN_POINT('Ctrl Pts',(0.205091310995403,0.928737319138035,
2.3769938343437));
#18558=CARTESIAN_POINT('Ctrl Pts',(0.193383491552286,0.931180374453942,
2.43471106618067));
#18559=CARTESIAN_POINT('Ctrl Pts',(0.156163794256122,0.937706308072193,
2.4861140371438));
#18560=CARTESIAN_POINT('Ctrl Pts',(0.127220061761462,0.941655887843543,
2.51114315400046));
#18561=CARTESIAN_POINT('Ctrl Pts',(0.105719704638418,0.944293922425639,
2.52657248312153));
#18562=CARTESIAN_POINT('Ctrl Pts',(0.0642457540090459,0.948373608976796,
2.54780176858962));
#18563=CARTESIAN_POINT('Ctrl Pts',(0.0257051198214169,0.949999961273794,
2.55499982053709));
#18564=CARTESIAN_POINT('Ctrl Pts',(1.43126818176587E-6,0.949999999998922,
2.554999999995));
#18565=CARTESIAN_POINT('',(1.63052496528509E-6,0.972500000001548,2.57749999999709));
#18566=CARTESIAN_POINT('Ctrl Pts',(-0.157876674355192,0.987458837468451,
2.55));
#18567=CARTESIAN_POINT('Ctrl Pts',(-0.14679428096426,0.985294697406766,
2.55388665064189));
#18568=CARTESIAN_POINT('Ctrl Pts',(-0.135549889588828,0.983354421647031,
2.55740912752908));
#18569=CARTESIAN_POINT('Ctrl Pts',(-0.0935709003424397,0.977055328631449,
2.56892572544489));
#18570=CARTESIAN_POINT('Ctrl Pts',(-0.062201374246487,0.974161715360584,
2.57437596695135));
#18571=CARTESIAN_POINT('Ctrl Pts',(-0.024619403298166,0.972834706545006,
2.57687004873351));
#18572=CARTESIAN_POINT('Ctrl Pts',(-0.0189840464089389,0.972691422895011,
2.57713968402705));
#18573=CARTESIAN_POINT('Ctrl Pts',(-0.0105124985263454,0.972559701868467,
2.57738760007473));
#18574=CARTESIAN_POINT('Ctrl Pts',(-0.00768142954473445,0.972529696233088,
2.5774440907214));
#18575=CARTESIAN_POINT('Ctrl Pts',(-0.0032326711402507,0.972504563213093,
2.57749140831944));
#18576=CARTESIAN_POINT('Ctrl Pts',(-0.0016155351650678,0.972499996930093,
2.57750000577993));
#18577=CARTESIAN_POINT('Ctrl Pts',(1.63052496528509E-6,0.972500000001548,
2.57749999999708));
#18578=CARTESIAN_POINT('',(1.43126818176587E-6,0.949999999998922,2.554999999995));
#18579=CARTESIAN_POINT('Ctrl Pts',(1.63052496528509E-6,0.972500000001548,
2.57749999999709));
#18580=CARTESIAN_POINT('Ctrl Pts',(1.56410603744535E-6,0.965000000000673,
2.56999999999639));
#18581=CARTESIAN_POINT('Ctrl Pts',(1.49768710960561E-6,0.957499999999797,
2.5624999999957));
#18582=CARTESIAN_POINT('Ctrl Pts',(1.43126818176587E-6,0.949999999998922,
2.554999999995));
#18583=CARTESIAN_POINT('',(-3.4869210388678E-5,0.950019014087066,2.14494180214374));
#18584=CARTESIAN_POINT('Ctrl Pts',(1.43126818176587E-6,0.949999999998922,
2.554999999995));
#18585=CARTESIAN_POINT('Ctrl Pts',(-0.0256272820571188,0.950000038611092,
2.55500017892945));
#18586=CARTESIAN_POINT('Ctrl Pts',(-0.0770180954946874,0.947836654449066,
2.545491956117));
#18587=CARTESIAN_POINT('Ctrl Pts',(-0.122912016192401,0.942342690587028,
2.51623971854639));
#18588=CARTESIAN_POINT('Ctrl Pts',(-0.162273278240718,0.936710691441896,
2.47869732563017));
#18589=CARTESIAN_POINT('Ctrl Pts',(-0.190116748917708,0.931705920244711,
2.43873850533649));
#18590=CARTESIAN_POINT('Ctrl Pts',(-0.205180438332203,0.928732184994508,
2.37559643476243));
#18591=CARTESIAN_POINT('Ctrl Pts',(-0.2063281706048,0.928475438592001,2.31418526323498));
#18592=CARTESIAN_POINT('Ctrl Pts',(-0.184239643247193,0.932952809171462,
2.25049218467674));
#18593=CARTESIAN_POINT('Ctrl Pts',(-0.14553094537117,0.939236323471161,
2.20367459542476));
#18594=CARTESIAN_POINT('Ctrl Pts',(-0.100297800754953,0.945335204532955,
2.16670715064481));
#18595=CARTESIAN_POINT('Ctrl Pts',(-0.0465835707283805,0.949504783852479,
2.14738282011878));
#18596=CARTESIAN_POINT('Ctrl Pts',(-0.00936425895417839,0.950027004161095,
2.14491207293051));
#18597=CARTESIAN_POINT('Ctrl Pts',(-3.48692103886768E-5,0.950019014087066,
2.14494180214374));
#18598=CARTESIAN_POINT('Ctrl Pts',(-3.48692103886768E-5,0.950019014087066,
2.14494180214374));
#18599=CARTESIAN_POINT('Ctrl Pts',(0.00462828401910463,0.950015020370377,
2.14495666183772));
#18600=CARTESIAN_POINT('Ctrl Pts',(0.0163025714633961,0.949918483082405,
2.14539826893541));
#18601=CARTESIAN_POINT('Ctrl Pts',(0.0352153629354055,0.949440687181237,
2.14762723913071));
#18602=CARTESIAN_POINT('Ctrl Pts',(0.0780526805587212,0.947387432123376,
2.15736934465489));
#18603=CARTESIAN_POINT('Ctrl Pts',(0.118791192081503,0.942966542359005,
2.17967292326805));
#18604=CARTESIAN_POINT('Ctrl Pts',(0.160393955305448,0.936941762000965,
2.2197692915117));
#18605=CARTESIAN_POINT('Ctrl Pts',(0.178421760132616,0.933804534087895,
2.24615013735776));
#18606=CARTESIAN_POINT('Ctrl Pts',(0.199355148110418,0.929918951193924,
2.29392783383353));
#18607=CARTESIAN_POINT('Ctrl Pts',(0.205101073179634,0.928738263704097,
2.32281627503367));
#18608=CARTESIAN_POINT('Ctrl Pts',(0.205091310995403,0.928737319138035,
2.3769938343437));
#18609=CARTESIAN_POINT('Ctrl Pts',(0.193383491552286,0.931180374453942,
2.43471106618067));
#18610=CARTESIAN_POINT('Ctrl Pts',(0.156163794256122,0.937706308072193,
2.4861140371438));
#18611=CARTESIAN_POINT('Ctrl Pts',(0.127220061761462,0.941655887843543,
2.51114315400046));
#18612=CARTESIAN_POINT('Ctrl Pts',(0.105719704638418,0.944293922425639,
2.52657248312153));
#18613=CARTESIAN_POINT('Ctrl Pts',(0.0642457540090459,0.948373608976796,
2.54780176858962));
#18614=CARTESIAN_POINT('Ctrl Pts',(0.0257051198214169,0.949999961273794,
2.55499982053709));
#18615=CARTESIAN_POINT('Ctrl Pts',(1.43126818176587E-6,0.949999999998922,
2.554999999995));
#18616=CARTESIAN_POINT('Ctrl Pts',(1.63052496528509E-6,0.972500000001548,
2.57749999999708));
#18617=CARTESIAN_POINT('Ctrl Pts',(0.000580473862567526,0.972500001100936,
2.57749999792719));
#18618=CARTESIAN_POINT('Ctrl Pts',(0.00115932100720228,0.972500587629742,
2.5774988936244));
#18619=CARTESIAN_POINT('Ctrl Pts',(0.00414265020169645,0.972506627935274,
2.57748752117621));
#18620=CARTESIAN_POINT('Ctrl Pts',(0.00654688441943462,0.972521597304209,
2.57745933671442));
#18621=CARTESIAN_POINT('Ctrl Pts',(0.0128156465435042,0.972586968658231,
2.57733627628346));
#18622=CARTESIAN_POINT('Ctrl Pts',(0.0166786361769429,0.972653363288268,
2.57721129835072));
#18623=CARTESIAN_POINT('Ctrl Pts',(0.0281987946478794,0.972929256482295,
2.57669227394828));
#18624=CARTESIAN_POINT('Ctrl Pts',(0.0358422720486675,0.973215079278776,
2.57615478699383));
#18625=CARTESIAN_POINT('Ctrl Pts',(0.0623401377173534,0.974562717145952,
2.57362665221117));
#18626=CARTESIAN_POINT('Ctrl Pts',(0.0810078079633459,0.976141626745025,
2.57067014303824));
#18627=CARTESIAN_POINT('Ctrl Pts',(0.119336271682641,0.980686505593142,
2.56227318576719));
#18628=CARTESIAN_POINT('Ctrl Pts',(0.138835225480719,0.983740474395769,
2.55667793110024));
#18629=CARTESIAN_POINT('Ctrl Pts',(0.157876674355193,0.987458837468451,
2.55));
#18630=CARTESIAN_POINT('Origin',(4.31687996699442E-17,0.705,2.35));
#18631=CARTESIAN_POINT('',(-0.205,0.457138928554548,2.35));
#18632=CARTESIAN_POINT('',(-1.45611632917078E-17,0.501,2.145));
#18633=CARTESIAN_POINT('Ctrl Pts',(-0.205,0.457138928554548,2.35));
#18634=CARTESIAN_POINT('Ctrl Pts',(-0.205,0.457138928554548,2.37609072012547));
#18635=CARTESIAN_POINT('Ctrl Pts',(-0.199722778787908,0.459609069157102,
2.40367567964064));
#18636=CARTESIAN_POINT('Ctrl Pts',(-0.178715671123715,0.468177727272261,
2.45407202914948));
#18637=CARTESIAN_POINT('Ctrl Pts',(-0.162998335554875,0.474117890962222,
2.47691544473161));
#18638=CARTESIAN_POINT('Ctrl Pts',(-0.126935588134045,0.485018345626291,
2.51297819215244));
#18639=CARTESIAN_POINT('Ctrl Pts',(-0.104084611878653,0.490733376060334,
2.52871076670624));
#18640=CARTESIAN_POINT('Ctrl Pts',(-0.0536585253249438,0.498772107838147,
2.5497295887861));
#18641=CARTESIAN_POINT('Ctrl Pts',(-0.0260615896504234,0.501,2.555));
#18642=CARTESIAN_POINT('Ctrl Pts',(0.0260615896504235,0.501,2.555));
#18643=CARTESIAN_POINT('Ctrl Pts',(0.0536585253249439,0.498772107838147,
2.5497295887861));
#18644=CARTESIAN_POINT('Ctrl Pts',(0.104084611878653,0.490733376060334,
2.52871076670624));
#18645=CARTESIAN_POINT('Ctrl Pts',(0.126935588134046,0.485018345626291,
2.51297819215244));
#18646=CARTESIAN_POINT('Ctrl Pts',(0.162998335554875,0.474117890962221,
2.47691544473161));
#18647=CARTESIAN_POINT('Ctrl Pts',(0.178715671123715,0.468177727272261,
2.45407202914948));
#18648=CARTESIAN_POINT('Ctrl Pts',(0.199722778787908,0.459609069157102,
2.40367567964064));
#18649=CARTESIAN_POINT('Ctrl Pts',(0.205,0.457138928554548,2.37609072012547));
#18650=CARTESIAN_POINT('Ctrl Pts',(0.205,0.457138928554548,2.32390927987453));
#18651=CARTESIAN_POINT('Ctrl Pts',(0.199722778787908,0.459609069157102,
2.29632432035936));
#18652=CARTESIAN_POINT('Ctrl Pts',(0.178715671123715,0.468177727272261,
2.24592797085052));
#18653=CARTESIAN_POINT('Ctrl Pts',(0.162998335554875,0.474117890962221,
2.22308455526839));
#18654=CARTESIAN_POINT('Ctrl Pts',(0.126935588134045,0.485018345626291,
2.18702180784756));
#18655=CARTESIAN_POINT('Ctrl Pts',(0.104084611878653,0.490733376060334,
2.17128923329376));
#18656=CARTESIAN_POINT('Ctrl Pts',(0.0536585253249439,0.498772107838147,
2.1502704112139));
#18657=CARTESIAN_POINT('Ctrl Pts',(0.0260615896504234,0.501,2.145));
#18658=CARTESIAN_POINT('Ctrl Pts',(-3.46944695195361E-17,0.501,2.145));
#18659=CARTESIAN_POINT('Ctrl Pts',(-3.46944695195361E-17,0.501,2.145));
#18660=CARTESIAN_POINT('Ctrl Pts',(-0.0260615896504235,0.501,2.145));
#18661=CARTESIAN_POINT('Ctrl Pts',(-0.0536585253249439,0.498772107838147,
2.1502704112139));
#18662=CARTESIAN_POINT('Ctrl Pts',(-0.104084611878653,0.490733376060334,
2.17128923329376));
#18663=CARTESIAN_POINT('Ctrl Pts',(-0.126935588134045,0.485018345626291,
2.18702180784756));
#18664=CARTESIAN_POINT('Ctrl Pts',(-0.162998335554875,0.474117890962221,
2.22308455526839));
#18665=CARTESIAN_POINT('Ctrl Pts',(-0.178715671123715,0.468177727272261,
2.24592797085052));
#18666=CARTESIAN_POINT('Ctrl Pts',(-0.199722778787908,0.459609069157102,
2.29632432035936));
#18667=CARTESIAN_POINT('Ctrl Pts',(-0.205,0.457138928554548,2.32390927987453));
#18668=CARTESIAN_POINT('Ctrl Pts',(-0.205,0.457138928554548,2.35));
#18669=CARTESIAN_POINT('',(1.80635402874235E-17,0.705,2.145));
#18670=CARTESIAN_POINT('Origin',(0.,0.,2.575));
#18671=CARTESIAN_POINT('',(-0.95,-1.16341445918999E-16,2.6));
#18672=CARTESIAN_POINT('Origin',(0.,0.,2.6));
#18673=CARTESIAN_POINT('',(-0.975,-1.19403062916867E-16,2.575));
#18674=CARTESIAN_POINT('Ctrl Pts',(1.03743092372925,-0.292083537906633,
1.28318517918604));
#18675=CARTESIAN_POINT('Ctrl Pts',(1.23979244918951,-0.398891247467648,
1.53750926858099));
#18676=CARTESIAN_POINT('Ctrl Pts',(1.33623488367509,-0.594491629104928,
1.74606924121326));
#18677=CARTESIAN_POINT('Ctrl Pts',(1.32675822718598,-0.878884682818471,
1.90886509708283));
#18678=CARTESIAN_POINT('Ctrl Pts',(1.05199356151554,-0.294610685989129,
1.26845681306972));
#18679=CARTESIAN_POINT('Ctrl Pts',(1.25726427409018,-0.402631406009323,
1.51984840181958));
#18680=CARTESIAN_POINT('Ctrl Pts',(1.35531508433345,-0.600652305106672,
1.72608377212012));
#18681=CARTESIAN_POINT('Ctrl Pts',(1.34605472186502,-0.888971417088906,
1.88700775532559));
#18682=CARTESIAN_POINT('Ctrl Pts',(1.07830248703538,-0.30261409250914,1.241120378339));
#18683=CARTESIAN_POINT('Ctrl Pts',(1.28869195855348,-0.413428941810942,
1.48709498232077));
#18684=CARTESIAN_POINT('Ctrl Pts',(1.38909450341186,-0.616606838701699,
1.68880599613843));
#18685=CARTESIAN_POINT('Ctrl Pts',(1.3795008682383,-0.912150767476977,1.84625490381855));
#18686=CARTESIAN_POINT('Ctrl Pts',(1.13234954650476,-0.339741650892321,
1.18057861631985));
#18687=CARTESIAN_POINT('Ctrl Pts',(1.35241043892922,-0.460769919763724,
1.41443334405943));
#18688=CARTESIAN_POINT('Ctrl Pts',(1.45460182159639,-0.677140712937715,
1.60624291768871));
#18689=CARTESIAN_POINT('Ctrl Pts',(1.4388862517722,-0.989017806729689,1.7559174048444));
#18690=CARTESIAN_POINT('Ctrl Pts',(1.17040376051196,-0.384106544865054,
1.1340877844534));
#18691=CARTESIAN_POINT('Ctrl Pts',(1.39633768248716,-0.51607374181577,1.35876508657129));
#18692=CARTESIAN_POINT('Ctrl Pts',(1.49702742698244,-0.744159155535334,
1.54303391436826));
#18693=CARTESIAN_POINT('Ctrl Pts',(1.4722721909128,-1.06856709212992,1.68683916414419));
#18694=CARTESIAN_POINT('Ctrl Pts',(1.19569665581665,-0.420763908606184,
1.10166698368801));
#18695=CARTESIAN_POINT('Ctrl Pts',(1.42522258493376,-0.561378116697244,
1.3199705116299));
#18696=CARTESIAN_POINT('Ctrl Pts',(1.52373714690788,-0.79825366200197,1.49898794576061));
#18697=CARTESIAN_POINT('Ctrl Pts',(1.491240341739,-1.13139054452036,1.63871928608014));
#18698=CARTESIAN_POINT('',(1.04067701160391,-0.293809324770207,1.28727233489076));
#18699=CARTESIAN_POINT('',(1.19131159212569,-0.414490807021284,1.10727038327973));
#18700=CARTESIAN_POINT('Ctrl Pts',(1.04067701160391,-0.293809324770207,
1.28727233489076));
#18701=CARTESIAN_POINT('Ctrl Pts',(1.07291073821506,-0.299434836228389,
1.2547227402422));
#18702=CARTESIAN_POINT('Ctrl Pts',(1.09698565606019,-0.312686039747329,
1.22803799031313));
#18703=CARTESIAN_POINT('Ctrl Pts',(1.14435511150659,-0.354129853275147,
1.17079203987136));
#18704=CARTESIAN_POINT('Ctrl Pts',(1.1680017368876,-0.38029714786499,1.14052203161155));
#18705=CARTESIAN_POINT('Ctrl Pts',(1.19131159212569,-0.414490807021284,
1.10727038327973));
#18706=CARTESIAN_POINT('Ctrl Pts',(1.04067701160391,-0.293809324770207,
1.28727233489076));
#18707=CARTESIAN_POINT('Ctrl Pts',(1.12993947443311,-0.341610972564375,
1.39987124007464));
#18708=CARTESIAN_POINT('Ctrl Pts',(1.19835965101752,-0.406884846288962,
1.50346488650363));
#18709=CARTESIAN_POINT('Ctrl Pts',(1.30500348982786,-0.592356746173702,
1.715480776583));
#18710=CARTESIAN_POINT('Ctrl Pts',(1.33194693676576,-0.722011051157661,
1.81902921434248));
#18711=CARTESIAN_POINT('Ctrl Pts',(1.32676788217082,-0.878593860895847,
1.90869858745619));
#18712=CARTESIAN_POINT('Ctrl Pts',(1.19131159212569,-0.414490807021284,
1.10727038327973));
#18713=CARTESIAN_POINT('Ctrl Pts',(1.26101451903381,-0.455811744539446,
1.17697999301248));
#18714=CARTESIAN_POINT('Ctrl Pts',(1.3231563905114,-0.510390409161008,1.24430717677952));
#18715=CARTESIAN_POINT('Ctrl Pts',(1.42696598762934,-0.655828360684346,
1.37795460947454));
#18716=CARTESIAN_POINT('Ctrl Pts',(1.46323512106126,-0.744250824847066,
1.43952296396723));
#18717=CARTESIAN_POINT('Ctrl Pts',(1.49770211069246,-0.926020771798772,
1.54471868724305));
#18718=CARTESIAN_POINT('Ctrl Pts',(1.50135379887057,-1.01770953159263,1.59041399531289));
#18719=CARTESIAN_POINT('Ctrl Pts',(1.4914400228729,-1.11782012388912,1.63615580822897));
#18720=CARTESIAN_POINT('Ctrl Pts',(1.26214138440836,-0.114046207919,1.10192461715937));
#18721=CARTESIAN_POINT('Ctrl Pts',(1.51915795367952,-0.193872070477571,
1.32030517702043));
#18722=CARTESIAN_POINT('Ctrl Pts',(1.67285198321398,-0.39921550360964,1.49938098964775));
#18723=CARTESIAN_POINT('Ctrl Pts',(1.72322347301172,-0.730076507315206,
1.63915205504133));
#18724=CARTESIAN_POINT('Ctrl Pts',(1.23350917110672,-0.131128471412264,
1.12620814253777));
#18725=CARTESIAN_POINT('Ctrl Pts',(1.48384440470435,-0.213229856531407,
1.3493730700966));
#18726=CARTESIAN_POINT('Ctrl Pts',(1.63116936194582,-0.416549152036911,
1.53236753871639));
#18727=CARTESIAN_POINT('Ctrl Pts',(1.67535851585319,-0.74115396361005,1.67519578767207));
#18728=CARTESIAN_POINT('Ctrl Pts',(1.18566161414104,-0.154321672329429,
1.16792358645355));
#18729=CARTESIAN_POINT('Ctrl Pts',(1.42508536822677,-0.239112514228603,
1.39930746388997));
#18730=CARTESIAN_POINT('Ctrl Pts',(1.56242925297242,-0.438352145622168,
1.58908978141842));
#18731=CARTESIAN_POINT('Ctrl Pts',(1.59768412386216,-0.752201465653598,
1.73717464481022));
#18732=CARTESIAN_POINT('Ctrl Pts',(1.11989042845005,-0.172598846101517,
1.2281493040678));
#18733=CARTESIAN_POINT('Ctrl Pts',(1.34476711329974,-0.258281860114562,
1.47154499595952));
#18734=CARTESIAN_POINT('Ctrl Pts',(1.47038505632135,-0.450170312236593,
1.67113613169256));
#18735=CARTESIAN_POINT('Ctrl Pts',(1.49675459841166,-0.748265815679371,
1.82691733765972));
#18736=CARTESIAN_POINT('Ctrl Pts',(1.08406383481182,-0.17018101435307,1.26357751389222));
#18737=CARTESIAN_POINT('Ctrl Pts',(1.30156053800083,-0.253820963688729,
1.51402822523202));
#18738=CARTESIAN_POINT('Ctrl Pts',(1.42264323155934,-0.439852505027485,
1.71951214242024));
#18739=CARTESIAN_POINT('Ctrl Pts',(1.44728013834437,-0.728627336389036,
1.87982452105687));
#18740=CARTESIAN_POINT('Ctrl Pts',(1.06503024353735,-0.165188454635723,
1.28318566992362));
#18741=CARTESIAN_POINT('Ctrl Pts',(1.27879462627691,-0.246892212254839,
1.5375404757467));
#18742=CARTESIAN_POINT('Ctrl Pts',(1.39806529952135,-0.42950771085669,1.74612008846831));
#18743=CARTESIAN_POINT('Ctrl Pts',(1.42284226327066,-0.713034950441276,
1.90892450808844));
#18744=CARTESIAN_POINT('',(1.25585067703094,-0.117749801015233,1.10727038327973));
#18745=CARTESIAN_POINT('',(1.06845992077163,-0.166511139289343,1.28727233489076));
#18746=CARTESIAN_POINT('Ctrl Pts',(1.25585067703094,-0.117749801015232,
1.10727038327973));
#18747=CARTESIAN_POINT('Ctrl Pts',(1.23367823136722,-0.131623884554202,
1.12805083925442));
#18748=CARTESIAN_POINT('Ctrl Pts',(1.20873355917046,-0.144946380875744,
1.15131250789248));
#18749=CARTESIAN_POINT('Ctrl Pts',(1.16557150946412,-0.161532774289013,
1.19194777349469));
#18750=CARTESIAN_POINT('Ctrl Pts',(1.14529581701501,-0.168037493511604,
1.21108489279932));
#18751=CARTESIAN_POINT('Ctrl Pts',(1.11004996015815,-0.172484956391328,
1.24526606650747));
#18752=CARTESIAN_POINT('Ctrl Pts',(1.09154853530975,-0.172587502434263,
1.26352342884154));
#18753=CARTESIAN_POINT('Ctrl Pts',(1.06845992077163,-0.166511139289343,
1.28727233489076));
#18754=CARTESIAN_POINT('Ctrl Pts',(1.71930883511106,-0.719647344681869,
1.63615580822897));
#18755=CARTESIAN_POINT('Ctrl Pts',(1.70798257074607,-0.634377380847188,
1.59808263051822));
#18756=CARTESIAN_POINT('Ctrl Pts',(1.68649822169668,-0.55237815462213,1.55687869031203));
#18757=CARTESIAN_POINT('Ctrl Pts',(1.61179111914083,-0.383878819109612,
1.4528510278119));
#18758=CARTESIAN_POINT('Ctrl Pts',(1.55475212125011,-0.306551362590219,
1.3904370872311));
#18759=CARTESIAN_POINT('Ctrl Pts',(1.41508721860523,-0.186091644383525,
1.25222975809873));
#18760=CARTESIAN_POINT('Ctrl Pts',(1.33721040532788,-0.145146699351923,
1.18062438818012));
#18761=CARTESIAN_POINT('Ctrl Pts',(1.25585067703094,-0.117749801015232,
1.10727038327973));
#18762=CARTESIAN_POINT('Ctrl Pts',(1.06845992077163,-0.166511139289343,
1.28727233489076));
#18763=CARTESIAN_POINT('Ctrl Pts',(1.16282366323453,-0.203229920731113,
1.39987124007464));
#18764=CARTESIAN_POINT('Ctrl Pts',(1.23859785430383,-0.259800859583567,
1.50346488650363));
#18765=CARTESIAN_POINT('Ctrl Pts',(1.36677481743678,-0.431100013478375,
1.715480776583));
#18766=CARTESIAN_POINT('Ctrl Pts',(1.40911659430225,-0.556572568507924,
1.81902921434248));
#18767=CARTESIAN_POINT('Ctrl Pts',(1.42280782457595,-0.712641620935351,
1.90869858745619));
#18768=CARTESIAN_POINT('Ctrl Pts',(1.06845992077163,-0.166511139289343,
1.28727233489076));
#18769=CARTESIAN_POINT('Ctrl Pts',(1.28063005644821,-0.24907069698643,1.54044293163017));
#18770=CARTESIAN_POINT('Ctrl Pts',(1.3988219960746,-0.431991468445895,1.74808806329354));
#18771=CARTESIAN_POINT('Ctrl Pts',(1.42303573965083,-0.715273453667736,
1.91020772988088));
#18772=CARTESIAN_POINT('Ctrl Pts',(1.05919895104906,-0.208943867782964,
1.28727233489076));
#18773=CARTESIAN_POINT('Ctrl Pts',(1.26754579908091,-0.299809769973181,
1.54044293163017));
#18774=CARTESIAN_POINT('Ctrl Pts',(1.37811826912839,-0.487026359393917,
1.74808806329354));
#18775=CARTESIAN_POINT('Ctrl Pts',(1.39091636119152,-0.770593636045173,
1.91020772988088));
#18776=CARTESIAN_POINT('Ctrl Pts',(1.04993798132648,-0.251376596276586,
1.28727233489076));
#18777=CARTESIAN_POINT('Ctrl Pts',(1.25446154171361,-0.350548842959932,
1.54044293163017));
#18778=CARTESIAN_POINT('Ctrl Pts',(1.35741454218218,-0.54206125034194,1.74808806329354));
#18779=CARTESIAN_POINT('Ctrl Pts',(1.35879698273221,-0.825913818422611,
1.91020772988088));
#18780=CARTESIAN_POINT('Ctrl Pts',(1.04067701160391,-0.293809324770207,
1.28727233489076));
#18781=CARTESIAN_POINT('Ctrl Pts',(1.24137728434631,-0.401287915946682,
1.54044293163017));
#18782=CARTESIAN_POINT('Ctrl Pts',(1.33671081523597,-0.597096141289963,
1.74808806329354));
#18783=CARTESIAN_POINT('Ctrl Pts',(1.3266776042729,-0.881234000800048,1.91020772988088));
#18784=CARTESIAN_POINT('Ctrl Pts',(1.06845992077163,-0.166511139289343,
1.28727233489076));
#18785=CARTESIAN_POINT('Ctrl Pts',(1.06442058969234,-0.187915337510243,
1.28796759655004));
#18786=CARTESIAN_POINT('Ctrl Pts',(1.06007279171241,-0.209261745030532,
1.2883190755065));
#18787=CARTESIAN_POINT('Ctrl Pts',(1.05542181279351,-0.230552888394581,
1.288319084765));
#18788=CARTESIAN_POINT('Ctrl Pts',(1.05079951139633,-0.251712752465176,
1.28831909396641));
#18789=CARTESIAN_POINT('Ctrl Pts',(1.0458824320276,-0.272796801398346,1.28797193184368));
#18790=CARTESIAN_POINT('Ctrl Pts',(1.04067701160391,-0.293809324770207,
1.28727233489076));
#18791=CARTESIAN_POINT('Origin',(0.,0.,1.37171309575435));
#18792=CARTESIAN_POINT('',(1.26108935601086,-0.0260686553993152,1.10727038327973));
#18793=CARTESIAN_POINT('Origin',(0.,0.,1.10727038327973));
#18794=CARTESIAN_POINT('Ctrl Pts',(1.26108935601086,-0.0260686553993151,
1.10727038327973));
#18795=CARTESIAN_POINT('Ctrl Pts',(1.34014965076829,-0.0438278133131022,
1.17697999301248));
#18796=CARTESIAN_POINT('Ctrl Pts',(1.41611581747018,-0.0765323136032893,
1.24430717677952));
#18797=CARTESIAN_POINT('Ctrl Pts',(1.55978740991095,-0.182773095427518,
1.37795460947453));
#18798=CARTESIAN_POINT('Ctrl Pts',(1.62160544971255,-0.255660077554628,
1.43952296396723));
#18799=CARTESIAN_POINT('Ctrl Pts',(1.71055550747305,-0.417882684528603,
1.54471868724299));
#18800=CARTESIAN_POINT('Ctrl Pts',(1.74236185427981,-0.503955443296344,
1.59041399531284));
#18801=CARTESIAN_POINT('Ctrl Pts',(1.76386916735271,-0.602229799711921,
1.63615580822897));
#18802=CARTESIAN_POINT('Origin',(0.,0.,1.37171309575435));
#18803=CARTESIAN_POINT('',(1.15799828028598,-0.500065917147839,1.10727038327973));
#18804=CARTESIAN_POINT('Ctrl Pts',(1.4127766116927,-1.21572094522251,1.63615580822897));
#18805=CARTESIAN_POINT('Ctrl Pts',(1.42835456209775,-1.13112438230172,1.59808263051822));
#18806=CARTESIAN_POINT('Ctrl Pts',(1.4332608863651,-1.04649945489987,1.55687869031203));
#18807=CARTESIAN_POINT('Ctrl Pts',(1.41427936788009,-0.863161299579018,
1.4528510278119));
#18808=CARTESIAN_POINT('Ctrl Pts',(1.38392755544946,-0.77199249847737,1.3904370872311));
#18809=CARTESIAN_POINT('Ctrl Pts',(1.2883224397548,-0.614269670090824,1.25222975809873));
#18810=CARTESIAN_POINT('Ctrl Pts',(1.22690987286759,-0.551263454538704,
1.18062438818012));
#18811=CARTESIAN_POINT('Ctrl Pts',(1.15799828028598,-0.500065917147839,
1.10727038327973));
#18812=CARTESIAN_POINT('Origin',(0.,0.,1.10727038327973));
#18813=CARTESIAN_POINT('Ctrl Pts',(0.896396663228496,-0.598371737951084,
1.28318517918604));
#18814=CARTESIAN_POINT('Ctrl Pts',(1.05584851328029,-0.762485056494508,
1.537509268581));
#18815=CARTESIAN_POINT('Ctrl Pts',(1.08712687701302,-0.9783144252754,1.74606924121326));
#18816=CARTESIAN_POINT('Ctrl Pts',(0.99023175442669,-1.24585984429376,1.90886509708284));
#18817=CARTESIAN_POINT('Ctrl Pts',(0.909465623084801,-0.605275301161475,
1.26845681306972));
#18818=CARTESIAN_POINT('Ctrl Pts',(1.0713094336526,-0.771441249464594,1.51984840181958));
#18819=CARTESIAN_POINT('Ctrl Pts',(1.1033694726,-0.990069682591163,1.72608377212012));
#18820=CARTESIAN_POINT('Ctrl Pts',(1.00546683912554,-1.26141584343748,1.88700775532559));
#18821=CARTESIAN_POINT('Ctrl Pts',(0.932013737380385,-0.621016981690702,
1.24112031232197));
#18822=CARTESIAN_POINT('Ctrl Pts',(1.09786234356421,-0.791422088358105,
1.48709491630374));
#18823=CARTESIAN_POINT('Ctrl Pts',(1.13056538342229,-1.01568188386468,1.68880590632088));
#18824=CARTESIAN_POINT('Ctrl Pts',(1.03011319759961,-1.29379626687142,1.846254814001));
#18825=CARTESIAN_POINT('Ctrl Pts',(0.971942506168048,-0.673028944353636,
1.180578495595));
#18826=CARTESIAN_POINT('Ctrl Pts',(1.14383306000902,-0.856136223676185,
1.41443322333459));
#18827=CARTESIAN_POINT('Ctrl Pts',(1.17416051125987,-1.09349602729722,1.60624275382305));
#18828=CARTESIAN_POINT('Ctrl Pts',(1.06283879403329,-1.38525239147931,1.75591724097875));
#18829=CARTESIAN_POINT('Ctrl Pts',(0.994424673117317,-0.726981684724075,
1.13408778445339));
#18830=CARTESIAN_POINT('Ctrl Pts',(1.16852049530615,-0.922307368817382,
1.35876508657128));
#18831=CARTESIAN_POINT('Ctrl Pts',(1.19379986392408,-1.17034433001556,1.54303391436826));
#18832=CARTESIAN_POINT('Ctrl Pts',(1.07000866982979,-1.47122482340642,1.68683916414419));
#18833=CARTESIAN_POINT('Ctrl Pts',(1.00715189764781,-0.769660843866376,
1.101666983688));
#18834=CARTESIAN_POINT('Ctrl Pts',(1.18199184824263,-0.974320315501954,
1.31997051162989));
#18835=CARTESIAN_POINT('Ctrl Pts',(1.20248619530708,-1.23004502025839,1.4989879457606));
#18836=CARTESIAN_POINT('Ctrl Pts',(1.06863493884117,-1.53683495813569,1.63871928608013));
#18837=CARTESIAN_POINT('',(0.89895057878464,-0.601016155111926,1.28727233489076));
#18838=CARTESIAN_POINT('',(1.00491994924733,-0.762339710524743,1.10727038327973));
#18839=CARTESIAN_POINT('Ctrl Pts',(0.89895057878464,-0.601016155111926,
1.28727233489076));
#18840=CARTESIAN_POINT('Ctrl Pts',(0.927868295879504,-0.616327103756327,
1.25472274024279));
#18841=CARTESIAN_POINT('Ctrl Pts',(0.946670056291831,-0.636369305963266,
1.22803799031441));
#18842=CARTESIAN_POINT('Ctrl Pts',(0.978914242877883,-0.690422681629505,
1.17079203986898));
#18843=CARTESIAN_POINT('Ctrl Pts',(0.993317381309374,-0.722616466766505,
1.14052203160877));
#18844=CARTESIAN_POINT('Ctrl Pts',(1.00491994924733,-0.762339710524744,
1.10727038327973));
#18845=CARTESIAN_POINT('Ctrl Pts',(0.89895057878464,-0.601016155111926,
1.28727233489076));
#18846=CARTESIAN_POINT('Ctrl Pts',(0.969072704191387,-0.674061841710201,
1.39987124007464));
#18847=CARTESIAN_POINT('Ctrl Pts',(1.01397342270847,-0.757283981982513,
1.50346488650363));
#18848=CARTESIAN_POINT('Ctrl Pts',(1.05808377148838,-0.966632999495317,
1.715480776583));
#18849=CARTESIAN_POINT('Ctrl Pts',(1.04364312863621,-1.09826755410688,1.81902921434248));
#18850=CARTESIAN_POINT('Ctrl Pts',(0.990330805779365,-1.24558623976355,
1.90869858745619));
#18851=CARTESIAN_POINT('Ctrl Pts',(1.00491994924733,-0.762339710524743,
1.10727038327973));
#18852=CARTESIAN_POINT('Ctrl Pts',(1.05844250017153,-0.823177646383102,
1.17697999301248));
#18853=CARTESIAN_POINT('Ctrl Pts',(1.10067719707671,-0.894287935370966,
1.24430717677952));
#18854=CARTESIAN_POINT('Ctrl Pts',(1.1544631922219,-1.06468657657251,1.37795460947453));
#18855=CARTESIAN_POINT('Ctrl Pts',(1.16163314380192,-1.15998911590305,1.43952296396722));
#18856=CARTESIAN_POINT('Ctrl Pts',(1.13824319621308,-1.3435134939588,1.54471868724288));
#18857=CARTESIAN_POINT('Ctrl Pts',(1.113382773081,-1.43184312013692,1.59041399531273));
#18858=CARTESIAN_POINT('Ctrl Pts',(1.07301833748062,-1.52399042602929,1.63615580822897));
#18859=CARTESIAN_POINT('Ctrl Pts',(1.16512557173636,-0.498487526286222,
1.10192461715937));
#18860=CARTESIAN_POINT('Ctrl Pts',(1.38489530661629,-0.653828920782168,
1.32030517702043));
#18861=CARTESIAN_POINT('Ctrl Pts',(1.46761240439959,-0.89661619800095,1.49938098964775));
#18862=CARTESIAN_POINT('Ctrl Pts',(1.41327686508625,-1.22684935794257,1.63915205504132));
#18863=CARTESIAN_POINT('Ctrl Pts',(1.13261600897807,-0.505885883797788,
1.12620814253776));
#18864=CARTESIAN_POINT('Ctrl Pts',(1.34532824088583,-0.661326782584696,
1.3493730700966));
#18865=CARTESIAN_POINT('Ctrl Pts',(1.4226134838877,-0.90022083894692,1.53236753871639));
#18866=CARTESIAN_POINT('Ctrl Pts',(1.36433146342889,-1.22259355973874,1.67519578767206));
#18867=CARTESIAN_POINT('Ctrl Pts',(1.07994282031223,-0.513157335393556,
1.16792434557146));
#18868=CARTESIAN_POINT('Ctrl Pts',(1.28144653067711,-0.667784226973456,
1.39930822300789));
#18869=CARTESIAN_POINT('Ctrl Pts',(1.35050022373304,-0.899713500733374,
1.58909081893483));
#18870=CARTESIAN_POINT('Ctrl Pts',(1.28704482486114,-1.20909629592349,1.73717568232663));
#18871=CARTESIAN_POINT('Ctrl Pts',(1.01174252544333,-0.5102156806996,1.22815018770195));
#18872=CARTESIAN_POINT('Ctrl Pts',(1.19913545447318,-0.661195786769768,
1.47154587959366));
#18873=CARTESIAN_POINT('Ctrl Pts',(1.25930861084253,-0.882510125799204,
1.6711373385863));
#18874=CARTESIAN_POINT('Ctrl Pts',(1.19227095916867,-1.17416443346653,1.82691854455345));
#18875=CARTESIAN_POINT('Ctrl Pts',(0.978417148622633,-0.496845910594336,
1.26357751389222));
#18876=CARTESIAN_POINT('Ctrl Pts',(1.15942263970987,-0.643602406938538,
1.51402822523202));
#18877=CARTESIAN_POINT('Ctrl Pts',(1.21709221666582,-0.857945526599466,
1.71951214242024));
#18878=CARTESIAN_POINT('Ctrl Pts',(1.15128697696661,-1.14019993459331,1.87982452105687));
#18879=CARTESIAN_POINT('Ctrl Pts',(0.961857913410637,-0.486216000974361,
1.28318566992362));
#18880=CARTESIAN_POINT('Ctrl Pts',(1.13991207295831,-0.629977719122415,
1.5375404757467));
#18881=CARTESIAN_POINT('Ctrl Pts',(1.19691393144611,-0.840512044007265,
1.74612008846831));
#18882=CARTESIAN_POINT('Ctrl Pts',(1.13286348887405,-1.11781897562891,1.90892450808844));
#18883=CARTESIAN_POINT('',(0.964710998256926,-0.488533777383804,1.28727233489076));
#18884=CARTESIAN_POINT('Ctrl Pts',(1.15799828028598,-0.500065917147839,
1.10727038327973));
#18885=CARTESIAN_POINT('Ctrl Pts',(1.13262370376014,-0.506409292188322,
1.12805083925462));
#18886=CARTESIAN_POINT('Ctrl Pts',(1.10478303294976,-0.51137141150027,1.15131250789266));
#18887=CARTESIAN_POINT('Ctrl Pts',(1.0586080068788,-0.513808202166539,1.19194777349574));
#18888=CARTESIAN_POINT('Ctrl Pts',(1.03731460866957,-0.513729024230128,
1.21108489280018));
#18889=CARTESIAN_POINT('Ctrl Pts',(1.00241946522287,-0.507067244033001,
1.24526606650725));
#18890=CARTESIAN_POINT('Ctrl Pts',(0.984791876090065,-0.501447516417141,
1.2635234288413));
#18891=CARTESIAN_POINT('Ctrl Pts',(0.964710998256925,-0.488533777383804,
1.28727233489076));
#18892=CARTESIAN_POINT('Ctrl Pts',(0.964710998256926,-0.488533777383804,
1.28727233489076));
#18893=CARTESIAN_POINT('Ctrl Pts',(1.04310952295002,-0.552615413818275,
1.39987124007464));
#18894=CARTESIAN_POINT('Ctrl Pts',(1.09769367964031,-0.629833086622262,
1.50346488650363));
#18895=CARTESIAN_POINT('Ctrl Pts',(1.16666286599128,-0.832357123065218,
1.715480776583));
#18896=CARTESIAN_POINT('Ctrl Pts',(1.16815913695893,-0.964772942765737,
1.81902921434248));
#18897=CARTESIAN_POINT('Ctrl Pts',(1.13295228123076,-1.11743425489732,1.90869858745619));
#18898=CARTESIAN_POINT('Ctrl Pts',(0.964710998256925,-0.488533777383804,
1.28727233489076));
#18899=CARTESIAN_POINT('Ctrl Pts',(1.14098448197888,-0.632616760336964,
1.54044293163017));
#18900=CARTESIAN_POINT('Ctrl Pts',(1.19686606932897,-0.843108069941918,
1.74808806329354));
#18901=CARTESIAN_POINT('Ctrl Pts',(1.13235576030722,-1.12000770619867,1.91020772988088));
#18902=CARTESIAN_POINT('Ctrl Pts',(0.94279085843283,-0.526027903293178,
1.28727233489076));
#18903=CARTESIAN_POINT('Ctrl Pts',(1.11286137791709,-0.676829228446517,
1.54044293163017));
#18904=CARTESIAN_POINT('Ctrl Pts',(1.16016893831867,-0.889051558128351,
1.74808806329354));
#18905=CARTESIAN_POINT('Ctrl Pts',(1.08471353963759,-1.16269489233868,1.91020772988088));
#18906=CARTESIAN_POINT('Ctrl Pts',(0.920870718608735,-0.563522029202552,
1.28727233489076));
#18907=CARTESIAN_POINT('Ctrl Pts',(1.0847382738553,-0.72104169655607,1.54044293163017));
#18908=CARTESIAN_POINT('Ctrl Pts',(1.12347180730837,-0.934995046314783,
1.74808806329354));
#18909=CARTESIAN_POINT('Ctrl Pts',(1.03707131896797,-1.20538207847869,1.91020772988088));
#18910=CARTESIAN_POINT('Ctrl Pts',(0.89895057878464,-0.601016155111926,
1.28727233489076));
#18911=CARTESIAN_POINT('Ctrl Pts',(1.05661516979351,-0.765254164665624,
1.54044293163017));
#18912=CARTESIAN_POINT('Ctrl Pts',(1.08677467629807,-0.980938534501216,
1.74808806329354));
#18913=CARTESIAN_POINT('Ctrl Pts',(0.989429098298345,-1.2480692646187,1.91020772988088));
#18914=CARTESIAN_POINT('Ctrl Pts',(0.964710998256926,-0.488533777383804,
1.28727233489076));
#18915=CARTESIAN_POINT('Ctrl Pts',(0.954255105111264,-0.507642157628455,
1.28796759655004));
#18916=CARTESIAN_POINT('Ctrl Pts',(0.943523700818291,-0.52660025413621,
1.2883190755065));
#18917=CARTESIAN_POINT('Ctrl Pts',(0.932521031881151,-0.545412103245543,
1.288319084765));
#18918=CARTESIAN_POINT('Ctrl Pts',(0.921586204420597,-0.564107960168963,
1.28831909396641));
#18919=CARTESIAN_POINT('Ctrl Pts',(0.910394454615237,-0.582640621209125,
1.28797193184368));
#18920=CARTESIAN_POINT('Ctrl Pts',(0.89895057878464,-0.601016155111926,
1.28727233489076));
#18921=CARTESIAN_POINT('Origin',(0.,0.,1.37171309575435));
#18922=CARTESIAN_POINT('',(0.946792943618188,-0.833432097145897,1.10727038327973));
#18923=CARTESIAN_POINT('Ctrl Pts',(0.967951970128402,-1.59279130921887,
1.63615580822897));
#18924=CARTESIAN_POINT('Ctrl Pts',(1.00890925697988,-1.51714904820957,1.59808263051822));
#18925=CARTESIAN_POINT('Ctrl Pts',(1.03972598936032,-1.43818209714157,1.55687869031203));
#18926=CARTESIAN_POINT('Ctrl Pts',(1.07832809822747,-1.25795153804723,1.4528510278119));
#18927=CARTESIAN_POINT('Ctrl Pts',(1.07763451813115,-1.16186562982554,1.3904370872311));
#18928=CARTESIAN_POINT('Ctrl Pts',(1.03544768423091,-0.982318700621181,
1.25222975809873));
#18929=CARTESIAN_POINT('Ctrl Pts',(0.996510853667277,-0.903418701916906,
1.18062438818012));
#18930=CARTESIAN_POINT('Ctrl Pts',(0.946792943618189,-0.833432097145897,
1.10727038327973));
#18931=CARTESIAN_POINT('Origin',(0.,0.,1.10727038327973));
#18932=CARTESIAN_POINT('Ctrl Pts',(0.667616851768136,-0.846087143183836,
1.28318517918604));
#18933=CARTESIAN_POINT('Ctrl Pts',(0.76855076836202,-1.05144151564591,1.53750926858099));
#18934=CARTESIAN_POINT('Ctrl Pts',(0.731603317170575,-1.26637298918249,
1.74606924121325));
#18935=CARTESIAN_POINT('Ctrl Pts',(0.5567744981938,-1.4908815637936,1.90886509708283));
#18936=CARTESIAN_POINT('Ctrl Pts',(0.677912852846922,-0.856691352655136,
1.26845681306972));
#18937=CARTESIAN_POINT('Ctrl Pts',(0.780487361597373,-1.06473704847503,
1.51984840181957));
#18938=CARTESIAN_POINT('Ctrl Pts',(0.743418369261301,-1.28257214132251,
1.72608377212011));
#18939=CARTESIAN_POINT('Ctrl Pts',(0.566456856673054,-1.5103840982294,1.88700775532558));
#18940=CARTESIAN_POINT('Ctrl Pts',(0.694492950134683,-0.878631748253098,
1.24111924840996));
#18941=CARTESIAN_POINT('Ctrl Pts',(0.799566273875774,-1.0919466731633,1.48709385239173));
#18942=CARTESIAN_POINT('Ctrl Pts',(0.761367941758637,-1.31533666464121,
1.68880445881715));
#18943=CARTESIAN_POINT('Ctrl Pts',(0.579890165126716,-1.54879772833385,
1.84625336649728));
#18944=CARTESIAN_POINT('Ctrl Pts',(0.716394511678361,-0.940438249469774,
1.18057655035131));
#18945=CARTESIAN_POINT('Ctrl Pts',(0.82328888189397,-1.16770072295994,1.4144312780909));
#18946=CARTESIAN_POINT('Ctrl Pts',(0.778782224872496,-1.40281580396029,
1.60624011348192));
#18947=CARTESIAN_POINT('Ctrl Pts',(0.582751305549686,-1.64589229282023,
1.75591460063762));
#18948=CARTESIAN_POINT('Ctrl Pts',(0.721104370153831,-0.998694792103054,
1.1340877844534));
#18949=CARTESIAN_POINT('Ctrl Pts',(0.826320380483539,-1.23825912446582,
1.35876508657128));
#18950=CARTESIAN_POINT('Ctrl Pts',(0.7737148524921,-1.48196804720541,1.54303391436826));
#18951=CARTESIAN_POINT('Ctrl Pts',(0.56300524495508,-1.72986881834178,1.68683916414418));
#18952=CARTESIAN_POINT('Ctrl Pts',(0.720020094497306,-1.04321801318649,
1.10166698368801));
#18953=CARTESIAN_POINT('Ctrl Pts',(0.823059514024041,-1.29188925333649,
1.31997051162989));
#18954=CARTESIAN_POINT('Ctrl Pts',(0.763527516695654,-1.54143100170428,
1.4989879457606));
#18955=CARTESIAN_POINT('Ctrl Pts',(0.541424102512144,-1.79184325828986,
1.63871928608013));
#18956=CARTESIAN_POINT('',(0.669228599956957,-0.849391336665505,1.28727233489076));
#18957=CARTESIAN_POINT('',(0.720159740047643,-1.03556549162895,1.10727038327973));
#18958=CARTESIAN_POINT('Ctrl Pts',(0.669228599956957,-0.849391336665505,
1.28727233489076));
#18959=CARTESIAN_POINT('Ctrl Pts',(0.691999639905454,-0.872888980165437,
1.25472274024255));
#18960=CARTESIAN_POINT('Ctrl Pts',(0.70368779557681,-0.897760310667366,
1.22803799031372));
#18961=CARTESIAN_POINT('Ctrl Pts',(0.717650427656666,-0.959132127442248,
1.17079203987312));
#18962=CARTESIAN_POINT('Ctrl Pts',(0.721400199597647,-0.994201051127665,
1.14052203161312));
#18963=CARTESIAN_POINT('Ctrl Pts',(0.720159740047643,-1.03556549162895,
1.10727038327973));
#18964=CARTESIAN_POINT('Ctrl Pts',(0.669228599956957,-0.849391336665505,
1.28727233489076));
#18965=CARTESIAN_POINT('Ctrl Pts',(0.713346345736856,-0.940530841324424,
1.39987124007464));
#18966=CARTESIAN_POINT('Ctrl Pts',(0.730332411016459,-1.03355488521186,
1.50346488650363));
#18967=CARTESIAN_POINT('Ctrl Pts',(0.707591441492496,-1.2462884798982,1.715480776583));
#18968=CARTESIAN_POINT('Ctrl Pts',(0.653180259586497,-1.36701797678012,
1.81902921434248));
#18969=CARTESIAN_POINT('Ctrl Pts',(0.556953250077769,-1.49065195897357,
1.90869858745619));
#18970=CARTESIAN_POINT('Ctrl Pts',(0.720159740047643,-1.03556549162895,
1.10727038327973));
#18971=CARTESIAN_POINT('Ctrl Pts',(0.752262754789917,-1.10996518478287,
1.17697999301248));
#18972=CARTESIAN_POINT('Ctrl Pts',(0.770456050723178,-1.19064632759639,
1.24430717677952));
#18973=CARTESIAN_POINT('Ctrl Pts',(0.768953495941756,-1.36932585223819,
1.37795460947453));
#18974=CARTESIAN_POINT('Ctrl Pts',(0.746322420853231,-1.46217959017504,
1.43952296396723));
#18975=CARTESIAN_POINT('Ctrl Pts',(0.667365107081636,-1.62949375452171,
1.54471868724302));
#18976=CARTESIAN_POINT('Ctrl Pts',(0.616426084068086,-1.70581792784517,
1.59041399531287));
#18977=CARTESIAN_POINT('Ctrl Pts',(0.549562141057364,-1.78098192700405,
1.63615580822897));
#18978=CARTESIAN_POINT('Ctrl Pts',(0.954059150195613,-0.834133412413726,
1.10192461715937));
#18979=CARTESIAN_POINT('Ctrl Pts',(1.11506945780848,-1.04978444082665,1.32030517702044));
#18980=CARTESIAN_POINT('Ctrl Pts',(1.11871269798568,-1.30624985183955,1.49938098964776));
#18981=CARTESIAN_POINT('Ctrl Pts',(0.96498887072721,-1.60352964545243,1.63915205504134));
#18982=CARTESIAN_POINT('Ctrl Pts',(0.909786283922669,-0.830120410746054,
1.13430265099723));
#18983=CARTESIAN_POINT('Ctrl Pts',(1.06188151028184,-1.04296293472434,1.35904945381842));
#18984=CARTESIAN_POINT('Ctrl Pts',(1.06009689157698,-1.29220976330375,1.54337045304296));
#18985=CARTESIAN_POINT('Ctrl Pts',(0.904675898434802,-1.5779663580892,1.68721036521566));
#18986=CARTESIAN_POINT('Ctrl Pts',(0.852548363463457,-0.818798046722487,
1.18072883129925));
#18987=CARTESIAN_POINT('Ctrl Pts',(0.993250080255865,-1.02679776283204,
1.41464170568302));
#18988=CARTESIAN_POINT('Ctrl Pts',(0.985477438725562,-1.26592128430496,
1.60649360709678));
#18989=CARTESIAN_POINT('Ctrl Pts',(0.829299566756361,-1.53630097399698,
1.75619511453864));
#18990=CARTESIAN_POINT('Ctrl Pts',(0.79375614980161,-0.790019116961202,
1.24117993109554));
#18991=CARTESIAN_POINT('Ctrl Pts',(0.923395339954023,-0.989381722131547,
1.48719616792706));
#18992=CARTESIAN_POINT('Ctrl Pts',(0.911933272667177,-1.21574497056749,
1.68893589783145));
#18993=CARTESIAN_POINT('Ctrl Pts',(0.759379860065507,-1.46910775939894,
1.84640075134781));
#18994=CARTESIAN_POINT('Ctrl Pts',(0.773880188435137,-0.771069384901099,
1.26847955290007));
#18995=CARTESIAN_POINT('Ctrl Pts',(0.900255846614141,-0.96560832231481,
1.51990601315848));
#18996=CARTESIAN_POINT('Ctrl Pts',(0.888894517998789,-1.18631348684325,
1.72616419407532));
#18997=CARTESIAN_POINT('Ctrl Pts',(0.739946404362065,-1.43341713701446,
1.88709951781478));
#18998=CARTESIAN_POINT('Ctrl Pts',(0.764532229061142,-0.75964933747155,
1.28318566992362));
#18999=CARTESIAN_POINT('Ctrl Pts',(0.889446983704125,-0.951396617529428,
1.53754047574671));
#19000=CARTESIAN_POINT('Ctrl Pts',(0.878600288371208,-1.16924120209866,
1.74612008846832));
#19001=CARTESIAN_POINT('Ctrl Pts',(0.731992143062391,-1.41318309117925,
1.90892450808845));
#19002=CARTESIAN_POINT('',(0.766529441696069,-0.762735325532963,1.28727233489076));
#19003=CARTESIAN_POINT('Ctrl Pts',(0.946792943618188,-0.833432097145897,
1.10727038327973));
#19004=CARTESIAN_POINT('Ctrl Pts',(0.920700076576133,-0.831623829941914,
1.12805083925439));
#19005=CARTESIAN_POINT('Ctrl Pts',(0.892688645988321,-0.827739845433019,
1.15131250789245));
#19006=CARTESIAN_POINT('Ctrl Pts',(0.848020576826707,-0.815788503303615,
1.19194777349474));
#19007=CARTESIAN_POINT('Ctrl Pts',(0.827793819033383,-0.809133178696747,
1.2110848927993));
#19008=CARTESIAN_POINT('Ctrl Pts',(0.796665168763682,-0.792014256883214,
1.24526606650786));
#19009=CARTESIAN_POINT('Ctrl Pts',(0.781636926589614,-0.781222353702314,
1.26352342884187));
#19010=CARTESIAN_POINT('Ctrl Pts',(0.766529441696069,-0.762735325532963,
1.28727233489076));
#19011=CARTESIAN_POINT('Ctrl Pts',(0.766529441696069,-0.762735325532963,
1.28727233489076));
#19012=CARTESIAN_POINT('Ctrl Pts',(0.821288554787752,-0.847907059902912,
1.39987124007464));
#19013=CARTESIAN_POINT('Ctrl Pts',(0.849339599532016,-0.938212862837218,
1.50346488650363));
#19014=CARTESIAN_POINT('Ctrl Pts',(0.852349824604395,-1.15213731807335,
1.715480776583));
#19015=CARTESIAN_POINT('Ctrl Pts',(0.812854124246772,-1.27853461941729,
1.81902921434248));
#19016=CARTESIAN_POINT('Ctrl Pts',(0.732195474855992,-1.41284463836769,
1.90869858745619));
#19017=CARTESIAN_POINT('Ctrl Pts',(0.766529441696069,-0.762735325532963,
1.28727233489076));
#19018=CARTESIAN_POINT('Ctrl Pts',(0.889651396707116,-0.954237887485568,
1.54044293163017));
#19019=CARTESIAN_POINT('Ctrl Pts',(0.877752552661174,-1.17169537927269,
1.74808806329354));
#19020=CARTESIAN_POINT('Ctrl Pts',(0.730832909558242,-1.41510780089433,
1.91020772988088));
#19021=CARTESIAN_POINT('Ctrl Pts',(0.734095827783031,-0.791620662577143,
1.28727233489076));
#19022=CARTESIAN_POINT('Ctrl Pts',(0.849242331321591,-0.987595926292982,
1.54044293163017));
#19023=CARTESIAN_POINT('Ctrl Pts',(0.828654188454018,-1.20405019596674,
1.74808806329354));
#19024=CARTESIAN_POINT('Ctrl Pts',(0.672331399180314,-1.44098347159841,
1.91020772988088));
#19025=CARTESIAN_POINT('Ctrl Pts',(0.701662213869994,-0.820505999621324,
1.28727233489076));
#19026=CARTESIAN_POINT('Ctrl Pts',(0.808833265936067,-1.0209539651004,1.54044293163017));
#19027=CARTESIAN_POINT('Ctrl Pts',(0.779555824246863,-1.23640501266079,
1.74808806329354));
#19028=CARTESIAN_POINT('Ctrl Pts',(0.613829888802385,-1.4668591423025,1.91020772988088));
#19029=CARTESIAN_POINT('Ctrl Pts',(0.669228599956957,-0.849391336665505,
1.28727233489076));
#19030=CARTESIAN_POINT('Ctrl Pts',(0.768424200550542,-1.05431200390781,
1.54044293163017));
#19031=CARTESIAN_POINT('Ctrl Pts',(0.730457460039708,-1.26875982935484,
1.74808806329354));
#19032=CARTESIAN_POINT('Ctrl Pts',(0.555328378424456,-1.49273481300659,
1.91020772988088));
#19033=CARTESIAN_POINT('Ctrl Pts',(0.766529441696069,-0.762735325532963,
1.28727233489076));
#19034=CARTESIAN_POINT('Ctrl Pts',(0.750680482155633,-0.777677426407099,
1.28796759655004));
#19035=CARTESIAN_POINT('Ctrl Pts',(0.734615936171903,-0.792391461327318,
1.2883190755065));
#19036=CARTESIAN_POINT('Ctrl Pts',(0.718338595112193,-0.806882581321257,
1.288319084765));
#19037=CARTESIAN_POINT('Ctrl Pts',(0.702161618687534,-0.821284350360125,
1.28831909396641));
#19038=CARTESIAN_POINT('Ctrl Pts',(0.685790724894005,-0.835451517520009,
1.28797193184368));
#19039=CARTESIAN_POINT('Ctrl Pts',(0.669228599956957,-0.849391336665505,
1.28727233489076));
#19040=CARTESIAN_POINT('Origin',(0.,0.,1.37171309575435));
#19041=CARTESIAN_POINT('',(0.642908916934714,-1.08521613661244,1.10727038327973));
#19042=CARTESIAN_POINT('Ctrl Pts',(0.428377445609996,-1.81394816223928,
1.63615580822897));
#19043=CARTESIAN_POINT('Ctrl Pts',(0.490704884304682,-1.75466459467969,
1.59808263051822));
#19044=CARTESIAN_POINT('Ctrl Pts',(0.544415468320011,-1.68908545531116,
1.55687869031203));
#19045=CARTESIAN_POINT('Ctrl Pts',(0.636822561166698,-1.52960471530762,
1.4528510278119));
#19046=CARTESIAN_POINT('Ctrl Pts',(0.665855105856972,-1.43800725813253,
1.39043708723109));
#19047=CARTESIAN_POINT('Ctrl Pts',(0.681216094986276,-1.25421153251789,
1.25222975809872));
#19048=CARTESIAN_POINT('Ctrl Pts',(0.668566409010631,-1.16714103226326,
1.18062438818012));
#19049=CARTESIAN_POINT('Ctrl Pts',(0.642908916934714,-1.08521613661244,
1.10727038327973));
#19050=CARTESIAN_POINT('Origin',(0.,0.,1.10727038327973));
#19051=CARTESIAN_POINT('Ctrl Pts',(0.373486051296586,-1.01098164380599,
1.28318517918604));
#19052=CARTESIAN_POINT('Ctrl Pts',(0.40602191942841,-1.23747555342209,1.537509268581));
#19053=CARTESIAN_POINT('Ctrl Pts',(0.304465327263429,-1.43047014156898,
1.74606924121326));
#19054=CARTESIAN_POINT('Ctrl Pts',(0.0688162748016435,-1.58996540824669,
1.90886509708284));
#19055=CARTESIAN_POINT('Ctrl Pts',(0.379996173302724,-1.02423814947078,
1.26846828789983));
#19056=CARTESIAN_POINT('Ctrl Pts',(0.413260018127926,-1.25379621584498,
1.51986220127974));
#19057=CARTESIAN_POINT('Ctrl Pts',(0.310691453231357,-1.44951276533331,
1.72609931925976));
#19058=CARTESIAN_POINT('Ctrl Pts',(0.0719956513773653,-1.61148865224617,
1.88702478432129));
#19059=CARTESIAN_POINT('Ctrl Pts',(0.388981181049686,-1.05021098685512,
1.24114793592828));
#19060=CARTESIAN_POINT('Ctrl Pts',(0.422993564147048,-1.28554831174898,
1.48712868773117));
#19061=CARTESIAN_POINT('Ctrl Pts',(0.317635541875722,-1.48619594640544,
1.68884366634831));
#19062=CARTESIAN_POINT('Ctrl Pts',(0.072903703454065,-1.65214688300286,
1.84629652534568));
#19063=CARTESIAN_POINT('Ctrl Pts',(0.390726670926086,-1.11570416593892,
1.18065052582665));
#19064=CARTESIAN_POINT('Ctrl Pts',(0.422167036078159,-1.36485769647199,
1.41452066958594));
#19065=CARTESIAN_POINT('Ctrl Pts',(0.307195656373209,-1.57470193347747,
1.6063408569219));
#19066=CARTESIAN_POINT('Ctrl Pts',(0.0456677490292576,-1.74530108095235,
1.75602521756879));
#19067=CARTESIAN_POINT('Ctrl Pts',(0.377231702026725,-1.17251250338939,
1.13419834492992));
#19068=CARTESIAN_POINT('Ctrl Pts',(0.40328175100029,-1.43283860087531,1.35889748756926));
#19069=CARTESIAN_POINT('Ctrl Pts',(0.277966085037659,-1.64835039139677,
1.54318426643097));
#19070=CARTESIAN_POINT('Ctrl Pts',(0.00100075866861844,-1.81900536712134,
1.68700348817738));
#19071=CARTESIAN_POINT('Ctrl Pts',(0.362468171451202,-1.21448591285885,
1.10179959977345));
#19072=CARTESIAN_POINT('Ctrl Pts',(0.383640993960513,-1.48279448162749,
1.32012924726704));
#19073=CARTESIAN_POINT('Ctrl Pts',(0.249943984819035,-1.7017123916886,1.49916808705051));
#19074=CARTESIAN_POINT('Ctrl Pts',(-0.0386228559732302,-1.87123964304219,
1.63891611912388));
#19075=CARTESIAN_POINT('',(0.373997862975653,-1.01462217612883,1.28727233489076));
#19076=CARTESIAN_POINT('',(0.364905277844141,-1.20742290720348,1.10727038327973));
#19077=CARTESIAN_POINT('Ctrl Pts',(0.373997862975653,-1.01462217612883,
1.28727233489076));
#19078=CARTESIAN_POINT('Ctrl Pts',(0.388393237732386,-1.04400640142099,
1.25472274024223));
#19079=CARTESIAN_POINT('Ctrl Pts',(0.39182367054918,-1.07127228109936,1.22803799031322));
#19080=CARTESIAN_POINT('Ctrl Pts',(0.38613798841402,-1.13395503795985,1.17079203987176));
#19081=CARTESIAN_POINT('Ctrl Pts',(0.3788673400596,-1.16846630960495,1.14052203161198));
#19082=CARTESIAN_POINT('Ctrl Pts',(0.364905277844141,-1.20742290720348,
1.10727038327973));
#19083=CARTESIAN_POINT('Ctrl Pts',(0.373997862975653,-1.01462217612883,
1.28727233489076));
#19084=CARTESIAN_POINT('Ctrl Pts',(0.387792676785358,-1.11493412912611,
1.39987124007464));
#19085=CARTESIAN_POINT('Ctrl Pts',(0.375201374409042,-1.20865423507634,
1.50346488650363));
#19086=CARTESIAN_POINT('Ctrl Pts',(0.287835131123855,-1.40394856048621,
1.715480776583));
#19087=CARTESIAN_POINT('Ctrl Pts',(0.198779555753984,-1.50195515531182,
1.81902921434248));
#19088=CARTESIAN_POINT('Ctrl Pts',(0.0690572297370875,-1.58980227845634,
1.90869858745619));
#19089=CARTESIAN_POINT('Ctrl Pts',(0.364905277844141,-1.20742290720348,
1.10727038327973));
#19090=CARTESIAN_POINT('Ctrl Pts',(0.372446289646659,-1.2881015973139,1.17697999301248));
#19091=CARTESIAN_POINT('Ctrl Pts',(0.364817298041905,-1.3704559615559,1.24430717677952));
#19092=CARTESIAN_POINT('Ctrl Pts',(0.30817327386479,-1.53992597283257,1.37795460947453));
#19093=CARTESIAN_POINT('Ctrl Pts',(0.257956459417354,-1.62124173855645,
1.43952296396723));
#19094=CARTESIAN_POINT('Ctrl Pts',(0.127450637982166,-1.75990988600071,
1.54779670475201));
#19095=CARTESIAN_POINT('Ctrl Pts',(0.0535283678677317,-1.81609416413933,
1.5933649555937));
#19096=CARTESIAN_POINT('Ctrl Pts',(-0.02768902675717,-1.86363850813291,
1.63615580822897));
#19097=CARTESIAN_POINT('Ctrl Pts',(0.649602771712747,-1.08812850838495,
1.10192461715937));
#19098=CARTESIAN_POINT('Ctrl Pts',(0.736092841324625,-1.34297974552473,
1.32030517702044));
#19099=CARTESIAN_POINT('Ctrl Pts',(0.660305598163236,-1.58801866900221,
1.49938098964776));
#19100=CARTESIAN_POINT('Ctrl Pts',(0.422241042228578,-1.82324527881739,
1.63915205504134));
#19101=CARTESIAN_POINT('Ctrl Pts',(0.618953337525113,-1.07500526379447,
1.12620814253776));
#19102=CARTESIAN_POINT('Ctrl Pts',(0.699675280139884,-1.3257887054316,1.34937307009661));
#19103=CARTESIAN_POINT('Ctrl Pts',(0.621781951952735,-1.56448518294015,
1.5323675387164));
#19104=CARTESIAN_POINT('Ctrl Pts',(0.385144875912206,-1.79103288048414,
1.67519578767208));
#19105=CARTESIAN_POINT('Ctrl Pts',(0.57206528258633,-1.04992951600932,1.16792267552994));
#19106=CARTESIAN_POINT('Ctrl Pts',(0.644197802222636,-1.29346620831953,
1.39930655296637));
#19107=CARTESIAN_POINT('Ctrl Pts',(0.563737612015952,-1.52169008642819,
1.58908853641613));
#19108=CARTESIAN_POINT('Ctrl Pts',(0.330550471617951,-1.73468787786898,
1.73717339980793));
#19109=CARTESIAN_POINT('Ctrl Pts',(0.518619720423095,-1.00746259753274,
1.2281482344299));
#19110=CARTESIAN_POINT('Ctrl Pts',(0.581479904896343,-1.23975486922368,
1.47154392632162));
#19111=CARTESIAN_POINT('Ctrl Pts',(0.500074721257065,-1.45417148278635,
1.67113467075223));
#19112=CARTESIAN_POINT('Ctrl Pts',(0.274410020975479,-1.65072103116967,
1.82691587671939));
#19113=CARTESIAN_POINT('Ctrl Pts',(0.499517401914415,-0.977055955806949,
1.26357751389222));
#19114=CARTESIAN_POINT('Ctrl Pts',(0.559692616049942,-1.20217681362938,
1.51402822523203));
#19115=CARTESIAN_POINT('Ctrl Pts',(0.480360559198655,-1.40948136690307,
1.71951214242025));
#19116=CARTESIAN_POINT('Ctrl Pts',(0.261218023549733,-1.59915063028856,
1.87982452105689));
#19117=CARTESIAN_POINT('Ctrl Pts',(0.49236880332188,-0.958722904028868,
1.28318566992362));
#19118=CARTESIAN_POINT('Ctrl Pts',(0.551916626543442,-1.17968618624264,
1.53754047574671));
#19119=CARTESIAN_POINT('Ctrl Pts',(0.47428312750236,-1.38351688474614,1.74612008846832));
#19120=CARTESIAN_POINT('Ctrl Pts',(0.259468306198631,-1.57021499953937,
1.90892450808845));
#19121=CARTESIAN_POINT('',(0.493314642657339,-0.962275025729455,1.28727233489076));
#19122=CARTESIAN_POINT('Ctrl Pts',(0.642908916934714,-1.08521613661244,
1.10727038327973));
#19123=CARTESIAN_POINT('Ctrl Pts',(0.618651911002038,-1.07543323295697,
1.12805083925432));
#19124=CARTESIAN_POINT('Ctrl Pts',(0.593211674629804,-1.06308333609217,
1.15131250789245));
#19125=CARTESIAN_POINT('Ctrl Pts',(0.554422984205302,-1.03791374180364,
1.19194777349641));
#19126=CARTESIAN_POINT('Ctrl Pts',(0.537242802809869,-1.0253337400692,1.21108489280038));
#19127=CARTESIAN_POINT('Ctrl Pts',(0.512927734894523,-0.999433395982646,
1.24526606650702));
#19128=CARTESIAN_POINT('Ctrl Pts',(0.501969908730686,-0.984525703912059,
1.26352342884097));
#19129=CARTESIAN_POINT('Ctrl Pts',(0.493314642657339,-0.962275025729455,
1.28727233489076));
#19130=CARTESIAN_POINT('Ctrl Pts',(0.493314642657339,-0.962275025729455,
1.28727233489076));
#19131=CARTESIAN_POINT('Ctrl Pts',(0.519074140629024,-1.06019965524839,
1.39987124007464));
#19132=CARTESIAN_POINT('Ctrl Pts',(0.517846241724568,-1.15475382712427,
1.50346488650363));
#19133=CARTESIAN_POINT('Ctrl Pts',(0.454602843714801,-1.35913828497575,
1.715480776583));
#19134=CARTESIAN_POINT('Ctrl Pts',(0.377981286365636,-1.46714441944577,
1.81902921434248));
#19135=CARTESIAN_POINT('Ctrl Pts',(0.259766273896473,-1.5699559447672,1.90869858745619));
#19136=CARTESIAN_POINT('Ctrl Pts',(0.493314642657339,-0.962275025729455,
1.28727233489076));
#19137=CARTESIAN_POINT('Ctrl Pts',(0.551233034159898,-1.18245156164078,
1.54044293163017));
#19138=CARTESIAN_POINT('Ctrl Pts',(0.472718500477254,-1.38558898119851,
1.74808806329354));
#19139=CARTESIAN_POINT('Ctrl Pts',(0.257771041609407,-1.57168728440264,
1.91020772988088));
#19140=CARTESIAN_POINT('Ctrl Pts',(0.453542382763444,-0.979724075862581,
1.28727233489076));
#19141=CARTESIAN_POINT('Ctrl Pts',(0.502493528317088,-1.20168985388846,
1.54044293163017));
#19142=CARTESIAN_POINT('Ctrl Pts',(0.416024993050258,-1.4011880115129,1.74808806329354));
#19143=CARTESIAN_POINT('Ctrl Pts',(0.194136776962956,-1.57821854873589,
1.91020772988088));
#19144=CARTESIAN_POINT('Ctrl Pts',(0.413770122869548,-0.997173125995706,
1.28727233489076));
#19145=CARTESIAN_POINT('Ctrl Pts',(0.453754022474278,-1.22092814613614,
1.54044293163017));
#19146=CARTESIAN_POINT('Ctrl Pts',(0.359331485623264,-1.41678704182728,
1.74808806329354));
#19147=CARTESIAN_POINT('Ctrl Pts',(0.130502512316506,-1.58474981306913,
1.91020772988088));
#19148=CARTESIAN_POINT('Ctrl Pts',(0.373997862975653,-1.01462217612883,
1.28727233489076));
#19149=CARTESIAN_POINT('Ctrl Pts',(0.405014516631467,-1.24016643838382,
1.54044293163017));
#19150=CARTESIAN_POINT('Ctrl Pts',(0.302637978196268,-1.43238607214167,
1.74808806329354));
#19151=CARTESIAN_POINT('Ctrl Pts',(0.0668682476700559,-1.59128107740238,
1.91020772988088));
#19152=CARTESIAN_POINT('Ctrl Pts',(0.493314642657339,-0.962275025729455,
1.28727233489076));
#19153=CARTESIAN_POINT('Ctrl Pts',(0.473624023308131,-0.971588210291789,
1.28796759655004));
#19154=CARTESIAN_POINT('Ctrl Pts',(0.45379884532281,-0.980617871367766,
1.2883190755065));
#19155=CARTESIAN_POINT('Ctrl Pts',(0.433840171694363,-0.989369770455727,
1.288319084765));
#19156=CARTESIAN_POINT('Ctrl Pts',(0.414004561469677,-0.998067706113493,
1.28831909396641));
#19157=CARTESIAN_POINT('Ctrl Pts',(0.394057020835224,-1.00648259836303,
1.28797193184368));
#19158=CARTESIAN_POINT('Ctrl Pts',(0.373997862975653,-1.01462217612883,
1.28727233489076));
#19159=CARTESIAN_POINT('Origin',(0.,0.,1.37171309575435));
#19160=CARTESIAN_POINT('',(0.27609248605185,-1.23077165948193,1.10727038327973));
#19161=CARTESIAN_POINT('Ctrl Pts',(-0.153129647965883,-1.85754313061971,
1.63615580822897));
#19162=CARTESIAN_POINT('Ctrl Pts',(-0.0607713534907783,-1.81335940151627,
1.59083969670469));
#19163=CARTESIAN_POINT('Ctrl Pts',(0.0223614442500381,-1.75708539039456,
1.54129005514746));
#19164=CARTESIAN_POINT('Ctrl Pts',(0.159600739735624,-1.61733286423933,
1.42521036359322));
#19165=CARTESIAN_POINT('Ctrl Pts',(0.208550308549108,-1.53789592166465,
1.36183966503053));
#19166=CARTESIAN_POINT('Ctrl Pts',(0.264206681902337,-1.37907079095174,
1.23219371736399));
#19167=CARTESIAN_POINT('Ctrl Pts',(0.275306576910198,-1.30454791379682,
1.17031259812849));
#19168=CARTESIAN_POINT('Ctrl Pts',(0.27609248605185,-1.23077165948193,1.10727038327973));
#19169=CARTESIAN_POINT('Origin',(0.,0.,1.10727038327973));
#19170=CARTESIAN_POINT('Ctrl Pts',(0.0427958338937929,-1.07691421720911,
1.28318517918604));
#19171=CARTESIAN_POINT('Ctrl Pts',(0.00374881610008805,-1.30237686203014,
1.53750926858099));
#19172=CARTESIAN_POINT('Ctrl Pts',(-0.15247585021093,-1.45454290982716,
1.74606924121326));
#19173=CARTESIAN_POINT('Ctrl Pts',(-0.42587816503926,-1.53341236060018,
1.90886509708283));
#19174=CARTESIAN_POINT('Ctrl Pts',(0.044892475801183,-1.091545040475,1.26845681306972));
#19175=CARTESIAN_POINT('Ctrl Pts',(0.00559080476410136,-1.32014932750452,
1.51984840181958));
#19176=CARTESIAN_POINT('Ctrl Pts',(-0.152438895007653,-1.4745930125769,
1.72608377212011));
#19177=CARTESIAN_POINT('Ctrl Pts',(-0.429508274607606,-1.55488138991364,
1.88700775532559));
#19178=CARTESIAN_POINT('Ctrl Pts',(0.0454099470705952,-1.11904054473513,
1.24111941924412));
#19179=CARTESIAN_POINT('Ctrl Pts',(0.00503268467650687,-1.35337649424567,
1.4870940232259));
#19180=CARTESIAN_POINT('Ctrl Pts',(-0.157175625948469,-1.51165038249934,
1.68880469124906));
#19181=CARTESIAN_POINT('Ctrl Pts',(-0.441219201568131,-1.59385438982847,
1.84625359892918));
#19182=CARTESIAN_POINT('Ctrl Pts',(0.0267999250011405,-1.18191630764682,
1.1805768626608));
#19183=CARTESIAN_POINT('Ctrl Pts',(-0.0203022432084527,-1.42860644524988,
1.41443159040039));
#19184=CARTESIAN_POINT('Ctrl Pts',(-0.194505783955952,-1.59265822923791,
1.60624053738541));
#19185=CARTESIAN_POINT('Ctrl Pts',(-0.495974904441967,-1.67408715628731,
1.7559150245411));
#19186=CARTESIAN_POINT('Ctrl Pts',(-0.00363238016698598,-1.23181557314521,
1.1340877844534));
#19187=CARTESIAN_POINT('Ctrl Pts',(-0.0593232212680527,-1.48747160844963,
1.35876508657128));
#19188=CARTESIAN_POINT('Ctrl Pts',(-0.245130498049611,-1.65371551508435,
1.54303391436825));
#19189=CARTESIAN_POINT('Ctrl Pts',(-0.561310568731037,-1.73041945202573,
1.68683916414418));
#19190=CARTESIAN_POINT('Ctrl Pts',(-0.0306796703370996,-1.26719829440569,
1.101666983688));
#19191=CARTESIAN_POINT('Ctrl Pts',(-0.0934843164788986,-1.52894260490194,
1.31997051162989));
#19192=CARTESIAN_POINT('Ctrl Pts',(-0.288323673548522,-1.69583409006838,
1.4989879457606));
#19193=CARTESIAN_POINT('Ctrl Pts',(-0.61519774154597,-1.76787274990501,
1.63871928608013));
#19194=CARTESIAN_POINT('',(0.0421576093699568,-1.08053472770428,1.28727233489076));
#19195=CARTESIAN_POINT('',(-0.0260686553993151,-1.26108935601086,1.10727038327973));
#19196=CARTESIAN_POINT('Ctrl Pts',(0.0421576093699568,-1.08053472770428,
1.28727233489076));
#19197=CARTESIAN_POINT('Ctrl Pts',(0.0467681993550376,-1.11292920208489,
1.25472274024224));
#19198=CARTESIAN_POINT('Ctrl Pts',(0.0416051146519907,-1.13992065666392,
1.22803799031328));
#19199=CARTESIAN_POINT('Ctrl Pts',(0.0168276724834171,-1.19777852863149,
1.17079203987139));
#19200=CARTESIAN_POINT('Ctrl Pts',(-0.000751694447691145,-1.22835394451355,
1.14052203161161));
#19201=CARTESIAN_POINT('Ctrl Pts',(-0.0260686553993153,-1.26108935601086,
1.10727038327973));
#19202=CARTESIAN_POINT('Ctrl Pts',(0.0421576093699568,-1.08053472770428,
1.28727233489076));
#19203=CARTESIAN_POINT('Ctrl Pts',(0.0242791587196548,-1.18019989616608,
1.39987124007464));
#19204=CARTESIAN_POINT('Ctrl Pts',(-0.0166569869072259,-1.26544208722232,
1.50346488650363));
#19205=CARTESIAN_POINT('Ctrl Pts',(-0.160096487344471,-1.42418037408903,
1.715480776583));
#19206=CARTESIAN_POINT('Ctrl Pts',(-0.275079075974333,-1.48987049850469,
1.81902921434248));
#19207=CARTESIAN_POINT('Ctrl Pts',(-0.425598593400272,-1.53333167412,1.90869858745619));
#19208=CARTESIAN_POINT('Ctrl Pts',(-0.0260686553993153,-1.26108935601086,
1.10727038327973));
#19209=CARTESIAN_POINT('Ctrl Pts',(-0.0438278133131018,-1.34014965076829,
1.17697999301248));
#19210=CARTESIAN_POINT('Ctrl Pts',(-0.0765323136032887,-1.41611581747018,
1.24430717677952));
#19211=CARTESIAN_POINT('Ctrl Pts',(-0.182773095427517,-1.55978740991095,
1.37795460947453));
#19212=CARTESIAN_POINT('Ctrl Pts',(-0.255660077554626,-1.62160544971255,
1.43952296396722));
#19213=CARTESIAN_POINT('Ctrl Pts',(-0.417882684528454,-1.71055550747297,
1.54471868724289));
#19214=CARTESIAN_POINT('Ctrl Pts',(-0.503955443296138,-1.74236185427976,
1.59041399531274));
#19215=CARTESIAN_POINT('Ctrl Pts',(-0.602229799711922,-1.76386916735271,
1.63615580822897));
#19216=CARTESIAN_POINT('Ctrl Pts',(0.281756991007075,-1.23578335387376,
1.1017328493151));
#19217=CARTESIAN_POINT('Ctrl Pts',(0.285293785520307,-1.50493278576873,
1.32007563441911));
#19218=CARTESIAN_POINT('Ctrl Pts',(0.137495264840177,-1.71461214828354,
1.4991204904476));
#19219=CARTESIAN_POINT('Ctrl Pts',(-0.161638571033313,-1.86482144141821,
1.63886741740056));
#19220=CARTESIAN_POINT('Ctrl Pts',(0.2566193137444,-1.21381148288727,1.12604029619216));
#19221=CARTESIAN_POINT('Ctrl Pts',(0.25591920404824,-1.47730375097777,1.34917212439386));
#19222=CARTESIAN_POINT('Ctrl Pts',(0.108074844008921,-1.68029140190124,
1.5321393304303));
#19223=CARTESIAN_POINT('Ctrl Pts',(-0.187017052056851,-1.82267525691206,
1.67494641070563));
#19224=CARTESIAN_POINT('Ctrl Pts',(0.219711749650112,-1.17543855297397,
1.16779612397805));
#19225=CARTESIAN_POINT('Ctrl Pts',(0.21307065152042,-1.42937433465483,1.39915507862236));
#19226=CARTESIAN_POINT('Ctrl Pts',(0.0660178837300413,-1.62159457256362,
1.58891631513415));
#19227=CARTESIAN_POINT('Ctrl Pts',(-0.221600535375876,-1.7521395453745,
1.73698522631426));
#19228=CARTESIAN_POINT('Ctrl Pts',(0.181934739915364,-1.11847368101377,
1.22808906223353));
#19229=CARTESIAN_POINT('Ctrl Pts',(0.169938151077974,-1.35883455739468,
1.47147297599239));
#19230=CARTESIAN_POINT('Ctrl Pts',(0.0262526925971304,-1.53761229859012,
1.67105384595181));
#19231=CARTESIAN_POINT('Ctrl Pts',(-0.249117593166629,-1.65481713073797,
1.82682748557709));
#19232=CARTESIAN_POINT('Ctrl Pts',(0.173143664137204,-1.08361696356336,
1.26355539141207));
#19233=CARTESIAN_POINT('Ctrl Pts',(0.160806376565823,-1.31631931390947,
1.51400180025811));
#19234=CARTESIAN_POINT('Ctrl Pts',(0.0212938283898079,-1.48896648444243,
1.71948206324579));
#19235=CARTESIAN_POINT('Ctrl Pts',(-0.245739828560967,-1.6016350942056,
1.87979168962264));
#19236=CARTESIAN_POINT('Ctrl Pts',(0.172008888578299,-1.06394999292458,
1.28318566992362));
#19237=CARTESIAN_POINT('Ctrl Pts',(0.160360824547434,-1.29249985168946,
1.53754047574671));
#19238=CARTESIAN_POINT('Ctrl Pts',(0.0235398295887214,-1.46236429518572,
1.74612008846832));
#19239=CARTESIAN_POINT('Ctrl Pts',(-0.238454096297838,-1.57354332341337,
1.90892450808845));
#19240=CARTESIAN_POINT('',(0.171810769270086,-1.06762054184321,1.28727233489076));
#19241=CARTESIAN_POINT('Ctrl Pts',(0.27609248605185,-1.23077165948193,1.10727038327973));
#19242=CARTESIAN_POINT('Ctrl Pts',(0.256045785977557,-1.21397173814618,
1.12805083925441));
#19243=CARTESIAN_POINT('Ctrl Pts',(0.235667011409714,-1.19436482287745,
1.15131250789248));
#19244=CARTESIAN_POINT('Ctrl Pts',(0.206554607000121,-1.15844075168674,
1.19194777349574));
#19245=CARTESIAN_POINT('Ctrl Pts',(0.194102717857772,-1.14116749104435,
1.21108489279997));
#19246=CARTESIAN_POINT('Ctrl Pts',(0.178981360555582,-1.10902103082124,
1.2452660665067));
#19247=CARTESIAN_POINT('Ctrl Pts',(0.173166578774629,-1.09145681862846,
1.26352342884077));
#19248=CARTESIAN_POINT('Ctrl Pts',(0.171810769270086,-1.06762054184321,
1.28727233489076));
#19249=CARTESIAN_POINT('Ctrl Pts',(0.171810769270086,-1.06762054184321,
1.28727233489076));
#19250=CARTESIAN_POINT('Ctrl Pts',(0.166049132983329,-1.16871252149279,
1.39987124007464));
#19251=CARTESIAN_POINT('Ctrl Pts',(0.135662485730195,-1.25825944116939,
1.50346488650363));
#19252=CARTESIAN_POINT('Ctrl Pts',(0.0123561690781436,-1.43309732687145,
1.715480776583));
#19253=CARTESIAN_POINT('Ctrl Pts',(-0.0938909933754473,-1.51213990150266,
1.81902921434248));
#19254=CARTESIAN_POINT('Ctrl Pts',(-0.238090659850088,-1.57338902476662,
1.90869858745619));
#19255=CARTESIAN_POINT('Ctrl Pts',(0.171810769270086,-1.06762054184321,
1.28727233489076));
#19256=CARTESIAN_POINT('Ctrl Pts',(0.158856141562724,-1.29491863831812,
1.54044293163017));
#19257=CARTESIAN_POINT('Ctrl Pts',(0.0214114678431581,-1.46385147967852,
1.74808806329354));
#19258=CARTESIAN_POINT('Ctrl Pts',(-0.240523251888612,-1.5744190659244,
1.91020772988088));
#19259=CARTESIAN_POINT('Ctrl Pts',(0.128593049303376,-1.07192527046357,
1.28727233489076));
#19260=CARTESIAN_POINT('Ctrl Pts',(0.106557157682628,-1.2981540059198,1.54044293163017));
#19261=CARTESIAN_POINT('Ctrl Pts',(-0.0373276272898297,-1.46116778184124,
1.74808806329354));
#19262=CARTESIAN_POINT('Ctrl Pts',(-0.303061305613997,-1.56096659822788,
1.91020772988088));
#19263=CARTESIAN_POINT('Ctrl Pts',(0.0853753293366665,-1.07622999908393,
1.28727233489076));
#19264=CARTESIAN_POINT('Ctrl Pts',(0.054258173802532,-1.30138937352148,
1.54044293163017));
#19265=CARTESIAN_POINT('Ctrl Pts',(-0.0960667224228173,-1.45848408400396,
1.74808806329354));
#19266=CARTESIAN_POINT('Ctrl Pts',(-0.365599359339382,-1.54751413053135,
1.91020772988088));
#19267=CARTESIAN_POINT('Ctrl Pts',(0.0421576093699568,-1.08053472770428,
1.28727233489076));
#19268=CARTESIAN_POINT('Ctrl Pts',(0.00195918992243604,-1.30462474112317,
1.54044293163017));
#19269=CARTESIAN_POINT('Ctrl Pts',(-0.154805817555805,-1.45580038616668,
1.74808806329354));
#19270=CARTESIAN_POINT('Ctrl Pts',(-0.428137413064767,-1.53406166283483,
1.91020772988088));
#19271=CARTESIAN_POINT('Ctrl Pts',(0.171810769270086,-1.06762054184321,
1.28727233489076));
#19272=CARTESIAN_POINT('Ctrl Pts',(0.150205945126601,-1.0703931707,1.28796759655004));
#19273=CARTESIAN_POINT('Ctrl Pts',(0.128560761691038,-1.07285457179227,
1.2883190755065));
#19274=CARTESIAN_POINT('Ctrl Pts',(0.106874449528872,-1.07501055311346,
1.288319084765));
#19275=CARTESIAN_POINT('Ctrl Pts',(0.0853218532357676,-1.07715324084587,
1.28831909396641));
#19276=CARTESIAN_POINT('Ctrl Pts',(0.0637502700203705,-1.07899214990168,
1.28797193184368));
#19277=CARTESIAN_POINT('Ctrl Pts',(0.0421576093699568,-1.08053472770428,
1.28727233489076));
#19278=CARTESIAN_POINT('Origin',(0.,0.,1.37171309575435));
#19279=CARTESIAN_POINT('',(-0.117749801015232,-1.25585067703094,1.10727038327973));
#19280=CARTESIAN_POINT('Ctrl Pts',(-0.719647344681869,-1.71930883511106,
1.63615580822897));
#19281=CARTESIAN_POINT('Ctrl Pts',(-0.634377380847188,-1.70798257074607,
1.59808263051822));
#19282=CARTESIAN_POINT('Ctrl Pts',(-0.552378154622127,-1.68649822169668,
1.55687869031203));
#19283=CARTESIAN_POINT('Ctrl Pts',(-0.383878819109611,-1.61179111914083,
1.4528510278119));
#19284=CARTESIAN_POINT('Ctrl Pts',(-0.306551362590219,-1.55475212125011,
1.3904370872311));
#19285=CARTESIAN_POINT('Ctrl Pts',(-0.186091644383524,-1.41508721860523,
1.25222975809872));
#19286=CARTESIAN_POINT('Ctrl Pts',(-0.145146699351922,-1.33721040532788,
1.18062438818012));
#19287=CARTESIAN_POINT('Ctrl Pts',(-0.117749801015232,-1.25585067703094,
1.10727038327973));
#19288=CARTESIAN_POINT('Origin',(0.,0.,1.10727038327973));
#19289=CARTESIAN_POINT('Ctrl Pts',(-0.292083537906633,-1.03743092372925,
1.28318517918604));
#19290=CARTESIAN_POINT('Ctrl Pts',(-0.398891247467646,-1.23979244918951,
1.53750926858099));
#19291=CARTESIAN_POINT('Ctrl Pts',(-0.594491629104921,-1.33623488367509,
1.74606924121325));
#19292=CARTESIAN_POINT('Ctrl Pts',(-0.878884682818457,-1.32675822718598,
1.90886509708283));
#19293=CARTESIAN_POINT('Ctrl Pts',(-0.294610685989129,-1.05199356151554,
1.26845681306972));
#19294=CARTESIAN_POINT('Ctrl Pts',(-0.402631406009321,-1.25726427409018,
1.51984840181957));
#19295=CARTESIAN_POINT('Ctrl Pts',(-0.600652305106666,-1.35531508433345,
1.72608377212011));
#19296=CARTESIAN_POINT('Ctrl Pts',(-0.888971417088892,-1.34605472186502,
1.88700775532558));
#19297=CARTESIAN_POINT('Ctrl Pts',(-0.302614092509142,-1.07830248703538,
1.241120378339));
#19298=CARTESIAN_POINT('Ctrl Pts',(-0.413428941810942,-1.28869195855348,
1.48709498232077));
#19299=CARTESIAN_POINT('Ctrl Pts',(-0.616606838701694,-1.38909450341185,
1.68880599613841));
#19300=CARTESIAN_POINT('Ctrl Pts',(-0.912150767476964,-1.3795008682383,
1.84625490381854));
#19301=CARTESIAN_POINT('Ctrl Pts',(-0.339741650892325,-1.13234954650477,
1.18057861631985));
#19302=CARTESIAN_POINT('Ctrl Pts',(-0.460769919763727,-1.35241043892923,
1.41443334405943));
#19303=CARTESIAN_POINT('Ctrl Pts',(-0.677140712937712,-1.4546018215964,
1.6062429176887));
#19304=CARTESIAN_POINT('Ctrl Pts',(-0.98901780672968,-1.43888625177221,
1.75591740484439));
#19305=CARTESIAN_POINT('Ctrl Pts',(-0.384106544865062,-1.17040376051197,
1.13408778445339));
#19306=CARTESIAN_POINT('Ctrl Pts',(-0.516073741815779,-1.39633768248717,
1.35876508657127));
#19307=CARTESIAN_POINT('Ctrl Pts',(-0.744159155535337,-1.49702742698244,
1.54303391436825));
#19308=CARTESIAN_POINT('Ctrl Pts',(-1.06856709212991,-1.4722721909128,1.68683916414418));
#19309=CARTESIAN_POINT('Ctrl Pts',(-0.420763908606196,-1.19569665581666,
1.101666983688));
#19310=CARTESIAN_POINT('Ctrl Pts',(-0.561378116697257,-1.42522258493377,
1.31997051162988));
#19311=CARTESIAN_POINT('Ctrl Pts',(-0.798253662001981,-1.52373714690789,
1.49898794576059));
#19312=CARTESIAN_POINT('Ctrl Pts',(-1.13139054452037,-1.49124034173901,
1.63871928608012));
#19313=CARTESIAN_POINT('',(-0.293809324770207,-1.04067701160391,1.28727233489076));
#19314=CARTESIAN_POINT('',(-0.414490807021284,-1.19131159212569,1.10727038327973));
#19315=CARTESIAN_POINT('Ctrl Pts',(-0.293809324770207,-1.04067701160391,
1.28727233489076));
#19316=CARTESIAN_POINT('Ctrl Pts',(-0.299434836228388,-1.07291073821506,
1.25472274024221));
#19317=CARTESIAN_POINT('Ctrl Pts',(-0.312686039747241,-1.09698565606009,
1.22803799031324));
#19318=CARTESIAN_POINT('Ctrl Pts',(-0.354129853274886,-1.14435511150628,
1.17079203987172));
#19319=CARTESIAN_POINT('Ctrl Pts',(-0.380297147864532,-1.16800173688728,
1.14052203161199));
#19320=CARTESIAN_POINT('Ctrl Pts',(-0.414490807021284,-1.19131159212569,
1.10727038327973));
#19321=CARTESIAN_POINT('Ctrl Pts',(-0.293809324770207,-1.04067701160391,
1.28727233489076));
#19322=CARTESIAN_POINT('Ctrl Pts',(-0.341610972564375,-1.12993947443311,
1.39987124007464));
#19323=CARTESIAN_POINT('Ctrl Pts',(-0.406884846288962,-1.19835965101752,
1.50346488650363));
#19324=CARTESIAN_POINT('Ctrl Pts',(-0.592356746173702,-1.30500348982786,
1.715480776583));
#19325=CARTESIAN_POINT('Ctrl Pts',(-0.722011051157661,-1.33194693676576,
1.81902921434248));
#19326=CARTESIAN_POINT('Ctrl Pts',(-0.878593860895847,-1.32676788217082,
1.90869858745619));
#19327=CARTESIAN_POINT('Ctrl Pts',(-0.414490807021284,-1.19131159212569,
1.10727038327973));
#19328=CARTESIAN_POINT('Ctrl Pts',(-0.455811744539447,-1.26101451903382,
1.17697999301248));
#19329=CARTESIAN_POINT('Ctrl Pts',(-0.510390409161016,-1.32315639051141,
1.24430717677953));
#19330=CARTESIAN_POINT('Ctrl Pts',(-0.655828360684357,-1.42696598762934,
1.37795460947454));
#19331=CARTESIAN_POINT('Ctrl Pts',(-0.744250824847073,-1.46323512106126,
1.43952296396723));
#19332=CARTESIAN_POINT('Ctrl Pts',(-0.926020771798391,-1.49770211069239,
1.54471868724282));
#19333=CARTESIAN_POINT('Ctrl Pts',(-1.01770953159214,-1.50135379887062,
1.59041399531267));
#19334=CARTESIAN_POINT('Ctrl Pts',(-1.11782012388912,-1.4914400228729,1.63615580822897));
#19335=CARTESIAN_POINT('Ctrl Pts',(-0.114046207919,-1.26214138440836,1.10192461715937));
#19336=CARTESIAN_POINT('Ctrl Pts',(-0.193872070477574,-1.51915795367953,
1.32030517702044));
#19337=CARTESIAN_POINT('Ctrl Pts',(-0.399215503609652,-1.67285198321399,
1.49938098964776));
#19338=CARTESIAN_POINT('Ctrl Pts',(-0.730076507315236,-1.72322347301172,
1.63915205504134));
#19339=CARTESIAN_POINT('Ctrl Pts',(-0.131128471412264,-1.23350917110671,
1.12620814253777));
#19340=CARTESIAN_POINT('Ctrl Pts',(-0.213229856531409,-1.48384440470435,
1.34937307009661));
#19341=CARTESIAN_POINT('Ctrl Pts',(-0.416549152036926,-1.63116936194583,
1.5323675387164));
#19342=CARTESIAN_POINT('Ctrl Pts',(-0.741153963610082,-1.67535851585319,
1.67519578767208));
#19343=CARTESIAN_POINT('Ctrl Pts',(-0.15432167232943,-1.18566161414104,
1.16792358645355));
#19344=CARTESIAN_POINT('Ctrl Pts',(-0.239112514228606,-1.42508536822678,
1.39930746388998));
#19345=CARTESIAN_POINT('Ctrl Pts',(-0.43835214562218,-1.56242925297243,
1.58908978141843));
#19346=CARTESIAN_POINT('Ctrl Pts',(-0.752201465653627,-1.59768412386216,
1.73717464481023));
#19347=CARTESIAN_POINT('Ctrl Pts',(-0.172598846101517,-1.11989042845005,
1.2281493040678));
#19348=CARTESIAN_POINT('Ctrl Pts',(-0.258281860114565,-1.34476711329974,
1.47154499595952));
#19349=CARTESIAN_POINT('Ctrl Pts',(-0.450170312236607,-1.47038505632136,
1.67113613169257));
#19350=CARTESIAN_POINT('Ctrl Pts',(-0.7482658156794,-1.49675459841166,1.82691733765973));
#19351=CARTESIAN_POINT('Ctrl Pts',(-0.17018101435307,-1.08406383481182,
1.26357751389222));
#19352=CARTESIAN_POINT('Ctrl Pts',(-0.253820963688731,-1.30156053800084,
1.51402822523203));
#19353=CARTESIAN_POINT('Ctrl Pts',(-0.439852505027495,-1.42264323155935,
1.71951214242026));
#19354=CARTESIAN_POINT('Ctrl Pts',(-0.728627336389063,-1.44728013834437,
1.87982452105689));
#19355=CARTESIAN_POINT('Ctrl Pts',(-0.165188454635723,-1.06503024353735,
1.28318566992362));
#19356=CARTESIAN_POINT('Ctrl Pts',(-0.246892212254841,-1.27879462627692,
1.53754047574671));
#19357=CARTESIAN_POINT('Ctrl Pts',(-0.429507710856701,-1.39806529952135,
1.74612008846832));
#19358=CARTESIAN_POINT('Ctrl Pts',(-0.713034950441302,-1.42284226327066,
1.90892450808846));
#19359=CARTESIAN_POINT('',(-0.166511139289342,-1.06845992077163,1.28727233489076));
#19360=CARTESIAN_POINT('Ctrl Pts',(-0.117749801015232,-1.25585067703094,
1.10727038327973));
#19361=CARTESIAN_POINT('Ctrl Pts',(-0.13162388455418,-1.23367823136726,
1.12805083925438));
#19362=CARTESIAN_POINT('Ctrl Pts',(-0.144946380875744,-1.20873355917046,
1.15131250789249));
#19363=CARTESIAN_POINT('Ctrl Pts',(-0.161532774289153,-1.16557150946376,
1.19194777349503));
#19364=CARTESIAN_POINT('Ctrl Pts',(-0.168037493511636,-1.14529581701476,
1.21108489279957));
#19365=CARTESIAN_POINT('Ctrl Pts',(-0.1724849563913,-1.11004996015836,1.24526606650726));
#19366=CARTESIAN_POINT('Ctrl Pts',(-0.172587502434316,-1.09154853530996,
1.26352342884133));
#19367=CARTESIAN_POINT('Ctrl Pts',(-0.166511139289342,-1.06845992077163,
1.28727233489076));
#19368=CARTESIAN_POINT('Ctrl Pts',(-0.166511139289342,-1.06845992077163,
1.28727233489076));
#19369=CARTESIAN_POINT('Ctrl Pts',(-0.203229920731113,-1.16282366323453,
1.39987124007464));
#19370=CARTESIAN_POINT('Ctrl Pts',(-0.259800859583567,-1.23859785430383,
1.50346488650363));
#19371=CARTESIAN_POINT('Ctrl Pts',(-0.431100013478375,-1.36677481743678,
1.715480776583));
#19372=CARTESIAN_POINT('Ctrl Pts',(-0.556572568507924,-1.40911659430225,
1.81902921434248));
#19373=CARTESIAN_POINT('Ctrl Pts',(-0.712641620935351,-1.42280782457595,
1.90869858745619));
#19374=CARTESIAN_POINT('Ctrl Pts',(-0.166511139289342,-1.06845992077163,
1.28727233489076));
#19375=CARTESIAN_POINT('Ctrl Pts',(-0.24907069698643,-1.28063005644821,
1.54044293163017));
#19376=CARTESIAN_POINT('Ctrl Pts',(-0.431991468445894,-1.3988219960746,
1.74808806329354));
#19377=CARTESIAN_POINT('Ctrl Pts',(-0.715273453667736,-1.42303573965083,
1.91020772988088));
#19378=CARTESIAN_POINT('Ctrl Pts',(-0.208943867782964,-1.05919895104906,
1.28727233489076));
#19379=CARTESIAN_POINT('Ctrl Pts',(-0.299809769973181,-1.26754579908091,
1.54044293163017));
#19380=CARTESIAN_POINT('Ctrl Pts',(-0.487026359393918,-1.37811826912839,
1.74808806329354));
#19381=CARTESIAN_POINT('Ctrl Pts',(-0.770593636045173,-1.39091636119152,
1.91020772988088));
#19382=CARTESIAN_POINT('Ctrl Pts',(-0.251376596276585,-1.04993798132648,
1.28727233489076));
#19383=CARTESIAN_POINT('Ctrl Pts',(-0.350548842959931,-1.25446154171361,
1.54044293163017));
#19384=CARTESIAN_POINT('Ctrl Pts',(-0.542061250341939,-1.35741454218218,
1.74808806329354));
#19385=CARTESIAN_POINT('Ctrl Pts',(-0.825913818422611,-1.35879698273221,
1.91020772988088));
#19386=CARTESIAN_POINT('Ctrl Pts',(-0.293809324770207,-1.04067701160391,
1.28727233489076));
#19387=CARTESIAN_POINT('Ctrl Pts',(-0.401287915946682,-1.24137728434631,
1.54044293163017));
#19388=CARTESIAN_POINT('Ctrl Pts',(-0.597096141289962,-1.33671081523597,
1.74808806329354));
#19389=CARTESIAN_POINT('Ctrl Pts',(-0.881234000800048,-1.3266776042729,
1.91020772988088));
#19390=CARTESIAN_POINT('Ctrl Pts',(-0.166511139289342,-1.06845992077163,
1.28727233489076));
#19391=CARTESIAN_POINT('Ctrl Pts',(-0.187915337510229,-1.06442058969234,
1.28796759655004));
#19392=CARTESIAN_POINT('Ctrl Pts',(-0.209261745030525,-1.06007279171241,
1.2883190755065));
#19393=CARTESIAN_POINT('Ctrl Pts',(-0.230552888394581,-1.05542181279351,
1.288319084765));
#19394=CARTESIAN_POINT('Ctrl Pts',(-0.251712752465177,-1.05079951139633,
1.28831909396641));
#19395=CARTESIAN_POINT('Ctrl Pts',(-0.272796801398346,-1.0458824320276,
1.28797193184368));
#19396=CARTESIAN_POINT('Ctrl Pts',(-0.293809324770207,-1.04067701160391,
1.28727233489076));
#19397=CARTESIAN_POINT('Origin',(0.,0.,1.37171309575435));
#19398=CARTESIAN_POINT('',(-0.500065917147839,-1.15799828028598,1.10727038327973));
#19399=CARTESIAN_POINT('Ctrl Pts',(-1.21572094522251,-1.4127766116927,1.63615580822897));
#19400=CARTESIAN_POINT('Ctrl Pts',(-1.13112438230172,-1.42835456209775,
1.59808263051822));
#19401=CARTESIAN_POINT('Ctrl Pts',(-1.04649945489987,-1.4332608863651,1.55687869031203));
#19402=CARTESIAN_POINT('Ctrl Pts',(-0.863161299579022,-1.41427936788009,
1.4528510278119));
#19403=CARTESIAN_POINT('Ctrl Pts',(-0.771992498477375,-1.38392755544946,
1.3904370872311));
#19404=CARTESIAN_POINT('Ctrl Pts',(-0.614269670090826,-1.2883224397548,
1.25222975809873));
#19405=CARTESIAN_POINT('Ctrl Pts',(-0.551263454538706,-1.22690987286759,
1.18062438818012));
#19406=CARTESIAN_POINT('Ctrl Pts',(-0.500065917147839,-1.15799828028598,
1.10727038327973));
#19407=CARTESIAN_POINT('Origin',(0.,0.,1.10727038327973));
#19408=CARTESIAN_POINT('Ctrl Pts',(-0.598371737951084,-0.896396663228496,
1.28318517918604));
#19409=CARTESIAN_POINT('Ctrl Pts',(-0.762485056494505,-1.05584851328028,
1.53750926858099));
#19410=CARTESIAN_POINT('Ctrl Pts',(-0.978314425275391,-1.08712687701302,
1.74606924121326));
#19411=CARTESIAN_POINT('Ctrl Pts',(-1.24585984429374,-0.990231754426695,
1.90886509708283));
#19412=CARTESIAN_POINT('Ctrl Pts',(-0.605275301161474,-0.9094656230848,
1.26845681306972));
#19413=CARTESIAN_POINT('Ctrl Pts',(-0.771441249464591,-1.0713094336526,
1.51984840181957));
#19414=CARTESIAN_POINT('Ctrl Pts',(-0.990069682591154,-1.1033694726,1.72608377212011));
#19415=CARTESIAN_POINT('Ctrl Pts',(-1.26141584343747,-1.00546683912554,
1.88700775532558));
#19416=CARTESIAN_POINT('Ctrl Pts',(-0.621016981690699,-0.932013737380383,
1.24112031232197));
#19417=CARTESIAN_POINT('Ctrl Pts',(-0.791422088358097,-1.09786234356421,
1.48709491630373));
#19418=CARTESIAN_POINT('Ctrl Pts',(-1.01568188386468,-1.13056538342228,
1.68880590632087));
#19419=CARTESIAN_POINT('Ctrl Pts',(-1.29379626687141,-1.03011319759961,
1.84625481400099));
#19420=CARTESIAN_POINT('Ctrl Pts',(-0.673028944353633,-0.971942506168048,
1.180578495595));
#19421=CARTESIAN_POINT('Ctrl Pts',(-0.856136223676178,-1.14383306000902,
1.41443322333459));
#19422=CARTESIAN_POINT('Ctrl Pts',(-1.0934960272972,-1.17416051125987,1.60624275382304));
#19423=CARTESIAN_POINT('Ctrl Pts',(-1.38525239147929,-1.0628387940333,1.75591724097873));
#19424=CARTESIAN_POINT('Ctrl Pts',(-0.726981684724073,-0.994424673117314,
1.1340877844534));
#19425=CARTESIAN_POINT('Ctrl Pts',(-0.922307368817375,-1.16852049530615,
1.35876508657128));
#19426=CARTESIAN_POINT('Ctrl Pts',(-1.17034433001555,-1.19379986392408,
1.54303391436826));
#19427=CARTESIAN_POINT('Ctrl Pts',(-1.4712248234064,-1.07000866982979,1.68683916414419));
#19428=CARTESIAN_POINT('Ctrl Pts',(-0.769660843866369,-1.00715189764781,
1.10166698368801));
#19429=CARTESIAN_POINT('Ctrl Pts',(-0.974320315501941,-1.18199184824263,
1.31997051162989));
#19430=CARTESIAN_POINT('Ctrl Pts',(-1.23004502025837,-1.20248619530708,
1.4989879457606));
#19431=CARTESIAN_POINT('Ctrl Pts',(-1.53683495813566,-1.06863493884117,
1.63871928608013));
#19432=CARTESIAN_POINT('',(-0.601016155111926,-0.89895057878464,1.28727233489076));
#19433=CARTESIAN_POINT('',(-0.762339710524743,-1.00491994924733,1.10727038327973));
#19434=CARTESIAN_POINT('Ctrl Pts',(-0.601016155111926,-0.89895057878464,
1.28727233489076));
#19435=CARTESIAN_POINT('Ctrl Pts',(-0.616327103756389,-0.927868295879621,
1.25472274024266));
#19436=CARTESIAN_POINT('Ctrl Pts',(-0.636369305963692,-0.946670056292108,
1.22803799031394));
#19437=CARTESIAN_POINT('Ctrl Pts',(-0.690422681628619,-0.978914242877335,
1.17079203986993));
#19438=CARTESIAN_POINT('Ctrl Pts',(-0.722616466765382,-0.993317381309037,
1.14052203160971));
#19439=CARTESIAN_POINT('Ctrl Pts',(-0.762339710524743,-1.00491994924733,
1.10727038327973));
#19440=CARTESIAN_POINT('Ctrl Pts',(-0.601016155111926,-0.89895057878464,
1.28727233489076));
#19441=CARTESIAN_POINT('Ctrl Pts',(-0.674061841710201,-0.969072704191387,
1.39987124007464));
#19442=CARTESIAN_POINT('Ctrl Pts',(-0.757283981982513,-1.01397342270847,
1.50346488650363));
#19443=CARTESIAN_POINT('Ctrl Pts',(-0.966632999495317,-1.05808377148838,
1.715480776583));
#19444=CARTESIAN_POINT('Ctrl Pts',(-1.09826755410688,-1.04364312863621,
1.81902921434248));
#19445=CARTESIAN_POINT('Ctrl Pts',(-1.24558623976355,-0.990330805779365,
1.90869858745619));
#19446=CARTESIAN_POINT('Ctrl Pts',(-0.762339710524744,-1.00491994924733,
1.10727038327973));
#19447=CARTESIAN_POINT('Ctrl Pts',(-0.823177646383102,-1.05844250017153,
1.17697999301248));
#19448=CARTESIAN_POINT('Ctrl Pts',(-0.894287935370968,-1.10067719707671,
1.24430717677952));
#19449=CARTESIAN_POINT('Ctrl Pts',(-1.06468657657252,-1.15446319222191,
1.37795460947454));
#19450=CARTESIAN_POINT('Ctrl Pts',(-1.15998911590306,-1.16163314380192,
1.43952296396723));
#19451=CARTESIAN_POINT('Ctrl Pts',(-1.343513493959,-1.13824319621306,1.544718687243));
#19452=CARTESIAN_POINT('Ctrl Pts',(-1.43184312013715,-1.1133827730809,1.59041399531284));
#19453=CARTESIAN_POINT('Ctrl Pts',(-1.5239904260293,-1.07301833748062,1.63615580822897));
#19454=CARTESIAN_POINT('Ctrl Pts',(-0.498487526286222,-1.16512557173636,
1.10192461715937));
#19455=CARTESIAN_POINT('Ctrl Pts',(-0.653828920782166,-1.38489530661629,
1.32030517702043));
#19456=CARTESIAN_POINT('Ctrl Pts',(-0.896616198000942,-1.46761240439959,
1.49938098964774));
#19457=CARTESIAN_POINT('Ctrl Pts',(-1.22684935794255,-1.41327686508626,
1.63915205504132));
#19458=CARTESIAN_POINT('Ctrl Pts',(-0.50588588379779,-1.13261600897808,
1.12620814253777));
#19459=CARTESIAN_POINT('Ctrl Pts',(-0.661326782584696,-1.34532824088583,
1.3493730700966));
#19460=CARTESIAN_POINT('Ctrl Pts',(-0.900220838946918,-1.42261348388769,
1.53236753871639));
#19461=CARTESIAN_POINT('Ctrl Pts',(-1.22259355973873,-1.3643314634289,1.67519578767207));
#19462=CARTESIAN_POINT('Ctrl Pts',(-0.513157335393553,-1.07994282031223,
1.16792434557146));
#19463=CARTESIAN_POINT('Ctrl Pts',(-0.667784226973451,-1.2814465306771,
1.39930822300788));
#19464=CARTESIAN_POINT('Ctrl Pts',(-0.89971350073337,-1.35050022373304,
1.58909081893482));
#19465=CARTESIAN_POINT('Ctrl Pts',(-1.20909629592348,-1.28704482486114,
1.73717568232662));
#19466=CARTESIAN_POINT('Ctrl Pts',(-0.5102156806996,-1.01174252544333,1.22815018770195));
#19467=CARTESIAN_POINT('Ctrl Pts',(-0.661195786769765,-1.19913545447318,
1.47154587959366));
#19468=CARTESIAN_POINT('Ctrl Pts',(-0.882510125799198,-1.25930861084253,
1.67113733858628));
#19469=CARTESIAN_POINT('Ctrl Pts',(-1.17416443346652,-1.19227095916867,
1.82691854455344));
#19470=CARTESIAN_POINT('Ctrl Pts',(-0.496845910594337,-0.978417148622633,
1.26357751389222));
#19471=CARTESIAN_POINT('Ctrl Pts',(-0.643602406938536,-1.15942263970987,
1.51402822523202));
#19472=CARTESIAN_POINT('Ctrl Pts',(-0.857945526599457,-1.21709221666582,
1.71951214242024));
#19473=CARTESIAN_POINT('Ctrl Pts',(-1.1401999345933,-1.15128697696661,1.87982452105687));
#19474=CARTESIAN_POINT('Ctrl Pts',(-0.486216000974361,-0.961857913410637,
1.28318566992362));
#19475=CARTESIAN_POINT('Ctrl Pts',(-0.629977719122413,-1.13991207295831,
1.5375404757467));
#19476=CARTESIAN_POINT('Ctrl Pts',(-0.840512044007258,-1.19691393144611,
1.7461200884683));
#19477=CARTESIAN_POINT('Ctrl Pts',(-1.1178189756289,-1.13286348887406,1.90892450808843));
#19478=CARTESIAN_POINT('',(-0.488533777383804,-0.964710998256926,1.28727233489076));
#19479=CARTESIAN_POINT('Ctrl Pts',(-0.500065917147839,-1.15799828028598,
1.10727038327973));
#19480=CARTESIAN_POINT('Ctrl Pts',(-0.506409292188217,-1.13262370376054,
1.12805083925429));
#19481=CARTESIAN_POINT('Ctrl Pts',(-0.511371411500259,-1.10478303295006,
1.15131250789239));
#19482=CARTESIAN_POINT('Ctrl Pts',(-0.513808202166494,-1.05860800687958,
1.19194777349505));
#19483=CARTESIAN_POINT('Ctrl Pts',(-0.513729024230272,-1.03731460867033,
1.21108489279944));
#19484=CARTESIAN_POINT('Ctrl Pts',(-0.507067244033084,-1.00241946522331,
1.24526606650682));
#19485=CARTESIAN_POINT('Ctrl Pts',(-0.501447516417348,-0.984791876090384,
1.26352342884092));
#19486=CARTESIAN_POINT('Ctrl Pts',(-0.488533777383804,-0.964710998256926,
1.28727233489076));
#19487=CARTESIAN_POINT('Ctrl Pts',(-0.488533777383804,-0.964710998256925,
1.28727233489076));
#19488=CARTESIAN_POINT('Ctrl Pts',(-0.552615413818275,-1.04310952295002,
1.39987124007464));
#19489=CARTESIAN_POINT('Ctrl Pts',(-0.629833086622262,-1.09769367964031,
1.50346488650363));
#19490=CARTESIAN_POINT('Ctrl Pts',(-0.832357123065218,-1.16666286599128,
1.715480776583));
#19491=CARTESIAN_POINT('Ctrl Pts',(-0.964772942765737,-1.16815913695893,
1.81902921434248));
#19492=CARTESIAN_POINT('Ctrl Pts',(-1.11743425489732,-1.13295228123076,
1.90869858745619));
#19493=CARTESIAN_POINT('Ctrl Pts',(-0.488533777383804,-0.964710998256926,
1.28727233489076));
#19494=CARTESIAN_POINT('Ctrl Pts',(-0.632616760336964,-1.14098448197888,
1.54044293163017));
#19495=CARTESIAN_POINT('Ctrl Pts',(-0.843108069941918,-1.19686606932897,
1.74808806329354));
#19496=CARTESIAN_POINT('Ctrl Pts',(-1.12000770619867,-1.13235576030722,
1.91020772988088));
#19497=CARTESIAN_POINT('Ctrl Pts',(-0.526027903293178,-0.94279085843283,
1.28727233489076));
#19498=CARTESIAN_POINT('Ctrl Pts',(-0.676829228446517,-1.11286137791709,
1.54044293163017));
#19499=CARTESIAN_POINT('Ctrl Pts',(-0.889051558128351,-1.16016893831867,
1.74808806329354));
#19500=CARTESIAN_POINT('Ctrl Pts',(-1.16269489233868,-1.08471353963759,
1.91020772988088));
#19501=CARTESIAN_POINT('Ctrl Pts',(-0.563522029202552,-0.920870718608735,
1.28727233489076));
#19502=CARTESIAN_POINT('Ctrl Pts',(-0.721041696556071,-1.0847382738553,
1.54044293163017));
#19503=CARTESIAN_POINT('Ctrl Pts',(-0.934995046314783,-1.12347180730837,
1.74808806329354));
#19504=CARTESIAN_POINT('Ctrl Pts',(-1.20538207847869,-1.03707131896797,
1.91020772988088));
#19505=CARTESIAN_POINT('Ctrl Pts',(-0.601016155111926,-0.89895057878464,
1.28727233489076));
#19506=CARTESIAN_POINT('Ctrl Pts',(-0.765254164665624,-1.05661516979351,
1.54044293163017));
#19507=CARTESIAN_POINT('Ctrl Pts',(-0.980938534501216,-1.08677467629807,
1.74808806329354));
#19508=CARTESIAN_POINT('Ctrl Pts',(-1.2480692646187,-0.989429098298345,
1.91020772988088));
#19509=CARTESIAN_POINT('Ctrl Pts',(-0.488533777383804,-0.964710998256926,
1.28727233489076));
#19510=CARTESIAN_POINT('Ctrl Pts',(-0.507642157628474,-0.954255105111254,
1.28796759655004));
#19511=CARTESIAN_POINT('Ctrl Pts',(-0.526600254136219,-0.943523700818285,
1.2883190755065));
#19512=CARTESIAN_POINT('Ctrl Pts',(-0.545412103245543,-0.932521031881151,
1.288319084765));
#19513=CARTESIAN_POINT('Ctrl Pts',(-0.564107960168956,-0.921586204420602,
1.28831909396641));
#19514=CARTESIAN_POINT('Ctrl Pts',(-0.58264062120911,-0.910394454615247,
1.28797193184368));
#19515=CARTESIAN_POINT('Ctrl Pts',(-0.601016155111926,-0.89895057878464,
1.28727233489076));
#19516=CARTESIAN_POINT('Origin',(0.,0.,1.37171309575435));
#19517=CARTESIAN_POINT('',(-0.833432097145896,-0.946792943618189,1.10727038327973));
#19518=CARTESIAN_POINT('Ctrl Pts',(-1.59279130921887,-0.967951970128403,
1.63615580822897));
#19519=CARTESIAN_POINT('Ctrl Pts',(-1.51714904820957,-1.00890925697988,
1.59808263051822));
#19520=CARTESIAN_POINT('Ctrl Pts',(-1.43818209714157,-1.03972598936032,
1.55687869031203));
#19521=CARTESIAN_POINT('Ctrl Pts',(-1.25795153804723,-1.07832809822747,
1.4528510278119));
#19522=CARTESIAN_POINT('Ctrl Pts',(-1.16186562982554,-1.07763451813115,
1.3904370872311));
#19523=CARTESIAN_POINT('Ctrl Pts',(-0.982318700621179,-1.03544768423091,
1.25222975809873));
#19524=CARTESIAN_POINT('Ctrl Pts',(-0.903418701916908,-0.996510853667279,
1.18062438818012));
#19525=CARTESIAN_POINT('Ctrl Pts',(-0.833432097145896,-0.946792943618189,
1.10727038327973));
#19526=CARTESIAN_POINT('Origin',(0.,0.,1.10727038327973));
#19527=CARTESIAN_POINT('Ctrl Pts',(-0.846087143183836,-0.667616851768136,
1.28318517918604));
#19528=CARTESIAN_POINT('Ctrl Pts',(-1.05144151564591,-0.768550768362021,
1.53750926858099));
#19529=CARTESIAN_POINT('Ctrl Pts',(-1.26637298918249,-0.731603317170575,
1.74606924121326));
#19530=CARTESIAN_POINT('Ctrl Pts',(-1.4908815637936,-0.556774498193799,
1.90886509708283));
#19531=CARTESIAN_POINT('Ctrl Pts',(-0.856691352655136,-0.677912852846922,
1.26845681306972));
#19532=CARTESIAN_POINT('Ctrl Pts',(-1.06473704847503,-0.780487361597375,
1.51984840181957));
#19533=CARTESIAN_POINT('Ctrl Pts',(-1.28257214132251,-0.743418369261301,
1.72608377212011));
#19534=CARTESIAN_POINT('Ctrl Pts',(-1.5103840982294,-0.566456856673053,
1.88700775532558));
#19535=CARTESIAN_POINT('Ctrl Pts',(-0.878631748253101,-0.694492950134682,
1.24111924840996));
#19536=CARTESIAN_POINT('Ctrl Pts',(-1.0919466731633,-0.799566273875773,
1.48709385239173));
#19537=CARTESIAN_POINT('Ctrl Pts',(-1.31533666464121,-0.761367941758639,
1.68880445881716));
#19538=CARTESIAN_POINT('Ctrl Pts',(-1.54879772833386,-0.579890165126717,
1.84625336649729));
#19539=CARTESIAN_POINT('Ctrl Pts',(-0.940438249469776,-0.716394511678365,
1.18057655035132));
#19540=CARTESIAN_POINT('Ctrl Pts',(-1.16770072295994,-0.823288881893975,
1.4144312780909));
#19541=CARTESIAN_POINT('Ctrl Pts',(-1.4028158039603,-0.778782224872495,
1.60624011348192));
#19542=CARTESIAN_POINT('Ctrl Pts',(-1.64589229282025,-0.582751305549683,
1.75591460063762));
#19543=CARTESIAN_POINT('Ctrl Pts',(-0.998694792103063,-0.721104370153831,
1.1340877844534));
#19544=CARTESIAN_POINT('Ctrl Pts',(-1.23825912446583,-0.826320380483539,
1.35876508657128));
#19545=CARTESIAN_POINT('Ctrl Pts',(-1.48196804720542,-0.773714852492101,
1.54303391436825));
#19546=CARTESIAN_POINT('Ctrl Pts',(-1.72986881834179,-0.563005244955079,
1.68683916414418));
#19547=CARTESIAN_POINT('Ctrl Pts',(-1.04321801318649,-0.720020094497307,
1.10166698368801));
#19548=CARTESIAN_POINT('Ctrl Pts',(-1.2918892533365,-0.823059514024041,
1.31997051162989));
#19549=CARTESIAN_POINT('Ctrl Pts',(-1.5414310017043,-0.763527516695652,
1.4989879457606));
#19550=CARTESIAN_POINT('Ctrl Pts',(-1.79184325828987,-0.541424102512139,
1.63871928608013));
#19551=CARTESIAN_POINT('',(-0.849391336665505,-0.669228599956957,1.28727233489076));
#19552=CARTESIAN_POINT('',(-1.03556549162895,-0.720159740047643,1.10727038327973));
#19553=CARTESIAN_POINT('Ctrl Pts',(-0.849391336665505,-0.669228599956957,
1.28727233489076));
#19554=CARTESIAN_POINT('Ctrl Pts',(-0.872888980165412,-0.69199963990543,
1.25472274024258));
#19555=CARTESIAN_POINT('Ctrl Pts',(-0.897760310667151,-0.70368779557676,
1.22803799031392));
#19556=CARTESIAN_POINT('Ctrl Pts',(-0.959132127442685,-0.717650427656767,
1.17079203987271));
#19557=CARTESIAN_POINT('Ctrl Pts',(-0.994201051128119,-0.721400199597632,
1.14052203161276));
#19558=CARTESIAN_POINT('Ctrl Pts',(-1.03556549162895,-0.720159740047643,
1.10727038327973));
#19559=CARTESIAN_POINT('Ctrl Pts',(-0.849391336665505,-0.669228599956957,
1.28727233489076));
#19560=CARTESIAN_POINT('Ctrl Pts',(-0.940530841324424,-0.713346345736856,
1.39987124007464));
#19561=CARTESIAN_POINT('Ctrl Pts',(-1.03355488521186,-0.73033241101646,
1.50346488650363));
#19562=CARTESIAN_POINT('Ctrl Pts',(-1.2462884798982,-0.707591441492497,
1.715480776583));
#19563=CARTESIAN_POINT('Ctrl Pts',(-1.36701797678012,-0.653180259586497,
1.81902921434248));
#19564=CARTESIAN_POINT('Ctrl Pts',(-1.49065195897357,-0.55695325007777,
1.90869858745619));
#19565=CARTESIAN_POINT('Ctrl Pts',(-1.03556549162895,-0.720159740047643,
1.10727038327973));
#19566=CARTESIAN_POINT('Ctrl Pts',(-1.10996518478287,-0.752262754789918,
1.17697999301248));
#19567=CARTESIAN_POINT('Ctrl Pts',(-1.19064632759639,-0.770456050723179,
1.24430717677953));
#19568=CARTESIAN_POINT('Ctrl Pts',(-1.36932585223819,-0.768953495941756,
1.37795460947454));
#19569=CARTESIAN_POINT('Ctrl Pts',(-1.46217959017504,-0.746322420853231,
1.43952296396723));
#19570=CARTESIAN_POINT('Ctrl Pts',(-1.62949375452151,-0.667365107081731,
1.5447186872429));
#19571=CARTESIAN_POINT('Ctrl Pts',(-1.70581792784496,-0.616426084068271,
1.59041399531275));
#19572=CARTESIAN_POINT('Ctrl Pts',(-1.78098192700405,-0.549562141057365,
1.63615580822897));
#19573=CARTESIAN_POINT('Ctrl Pts',(-0.834133412413726,-0.954059150195613,
1.10192461715937));
#19574=CARTESIAN_POINT('Ctrl Pts',(-1.04978444082665,-1.11506945780848,
1.32030517702043));
#19575=CARTESIAN_POINT('Ctrl Pts',(-1.30624985183955,-1.11871269798568,
1.49938098964775));
#19576=CARTESIAN_POINT('Ctrl Pts',(-1.60352964545242,-0.964988870727218,
1.63915205504133));
#19577=CARTESIAN_POINT('Ctrl Pts',(-0.830120410746055,-0.909786283922666,
1.13430265099723));
#19578=CARTESIAN_POINT('Ctrl Pts',(-1.04296293472434,-1.06188151028183,
1.35904945381841));
#19579=CARTESIAN_POINT('Ctrl Pts',(-1.29220976330374,-1.06009689157698,
1.54337045304295));
#19580=CARTESIAN_POINT('Ctrl Pts',(-1.57796635808919,-0.904675898434815,
1.68721036521564));
#19581=CARTESIAN_POINT('Ctrl Pts',(-0.818798046722494,-0.852548363463462,
1.18072883129925));
#19582=CARTESIAN_POINT('Ctrl Pts',(-1.02679776283204,-0.993250080255868,
1.41464170568302));
#19583=CARTESIAN_POINT('Ctrl Pts',(-1.26592128430496,-0.985477438725565,
1.60649360709678));
#19584=CARTESIAN_POINT('Ctrl Pts',(-1.53630097399697,-0.82929956675637,
1.75619511453864));
#19585=CARTESIAN_POINT('Ctrl Pts',(-0.790019116961201,-0.793756149801608,
1.24117993109554));
#19586=CARTESIAN_POINT('Ctrl Pts',(-0.989381722131543,-0.923395339954019,
1.48719616792706));
#19587=CARTESIAN_POINT('Ctrl Pts',(-1.21574497056748,-0.911933272667178,
1.68893589783144));
#19588=CARTESIAN_POINT('Ctrl Pts',(-1.46910775939892,-0.759379860065515,
1.84640075134779));
#19589=CARTESIAN_POINT('Ctrl Pts',(-0.771069384901098,-0.773880188435137,
1.26847955290007));
#19590=CARTESIAN_POINT('Ctrl Pts',(-0.965608322314806,-0.900255846614139,
1.51990601315847));
#19591=CARTESIAN_POINT('Ctrl Pts',(-1.18631348684325,-0.88889451799879,
1.72616419407531));
#19592=CARTESIAN_POINT('Ctrl Pts',(-1.43341713701445,-0.739946404362073,
1.88709951781477));
#19593=CARTESIAN_POINT('Ctrl Pts',(-0.75964933747155,-0.764532229061142,
1.28318566992362));
#19594=CARTESIAN_POINT('Ctrl Pts',(-0.951396617529425,-0.889446983704123,
1.5375404757467));
#19595=CARTESIAN_POINT('Ctrl Pts',(-1.16924120209865,-0.878600288371209,
1.74612008846831));
#19596=CARTESIAN_POINT('Ctrl Pts',(-1.41318309117923,-0.731992143062398,
1.90892450808844));
#19597=CARTESIAN_POINT('',(-0.762735325532963,-0.766529441696069,1.28727233489076));
#19598=CARTESIAN_POINT('Ctrl Pts',(-0.833432097145896,-0.946792943618189,
1.10727038327973));
#19599=CARTESIAN_POINT('Ctrl Pts',(-0.831623829941906,-0.920700076575993,
1.12805083925451));
#19600=CARTESIAN_POINT('Ctrl Pts',(-0.827739845432993,-0.892688645988233,
1.15131250789253));
#19601=CARTESIAN_POINT('Ctrl Pts',(-0.815788503303453,-0.848020576826098,
1.19194777349529));
#19602=CARTESIAN_POINT('Ctrl Pts',(-0.809133178696535,-0.827793819032994,
1.21108489279973));
#19603=CARTESIAN_POINT('Ctrl Pts',(-0.792014256883054,-0.796665168763393,
1.24526606650818));
#19604=CARTESIAN_POINT('Ctrl Pts',(-0.781222353702122,-0.781636926589459,
1.26352342884212));
#19605=CARTESIAN_POINT('Ctrl Pts',(-0.762735325532963,-0.766529441696069,
1.28727233489076));
#19606=CARTESIAN_POINT('Ctrl Pts',(-0.762735325532963,-0.766529441696069,
1.28727233489076));
#19607=CARTESIAN_POINT('Ctrl Pts',(-0.847907059902912,-0.821288554787752,
1.39987124007464));
#19608=CARTESIAN_POINT('Ctrl Pts',(-0.938212862837218,-0.849339599532016,
1.50346488650363));
#19609=CARTESIAN_POINT('Ctrl Pts',(-1.15213731807335,-0.852349824604395,
1.715480776583));
#19610=CARTESIAN_POINT('Ctrl Pts',(-1.27853461941729,-0.812854124246773,
1.81902921434248));
#19611=CARTESIAN_POINT('Ctrl Pts',(-1.41284463836769,-0.732195474855993,
1.90869858745619));
#19612=CARTESIAN_POINT('Ctrl Pts',(-0.762735325532963,-0.766529441696069,
1.28727233489076));
#19613=CARTESIAN_POINT('Ctrl Pts',(-0.954237887485567,-0.889651396707116,
1.54044293163017));
#19614=CARTESIAN_POINT('Ctrl Pts',(-1.17169537927269,-0.877752552661174,
1.74808806329354));
#19615=CARTESIAN_POINT('Ctrl Pts',(-1.41510780089433,-0.730832909558243,
1.91020772988088));
#19616=CARTESIAN_POINT('Ctrl Pts',(-0.791620662577143,-0.734095827783031,
1.28727233489076));
#19617=CARTESIAN_POINT('Ctrl Pts',(-0.987595926292982,-0.849242331321591,
1.54044293163017));
#19618=CARTESIAN_POINT('Ctrl Pts',(-1.20405019596674,-0.828654188454019,
1.74808806329354));
#19619=CARTESIAN_POINT('Ctrl Pts',(-1.44098347159841,-0.672331399180314,
1.91020772988088));
#19620=CARTESIAN_POINT('Ctrl Pts',(-0.820505999621324,-0.701662213869994,
1.28727233489076));
#19621=CARTESIAN_POINT('Ctrl Pts',(-1.0209539651004,-0.808833265936067,
1.54044293163017));
#19622=CARTESIAN_POINT('Ctrl Pts',(-1.23640501266079,-0.779555824246864,
1.74808806329354));
#19623=CARTESIAN_POINT('Ctrl Pts',(-1.4668591423025,-0.613829888802386,
1.91020772988088));
#19624=CARTESIAN_POINT('Ctrl Pts',(-0.849391336665505,-0.669228599956957,
1.28727233489076));
#19625=CARTESIAN_POINT('Ctrl Pts',(-1.05431200390781,-0.768424200550542,
1.54044293163017));
#19626=CARTESIAN_POINT('Ctrl Pts',(-1.26875982935484,-0.730457460039709,
1.74808806329354));
#19627=CARTESIAN_POINT('Ctrl Pts',(-1.49273481300659,-0.555328378424457,
1.91020772988088));
#19628=CARTESIAN_POINT('Ctrl Pts',(-0.762735325532963,-0.766529441696069,
1.28727233489076));
#19629=CARTESIAN_POINT('Ctrl Pts',(-0.777677426407099,-0.750680482155632,
1.28796759655004));
#19630=CARTESIAN_POINT('Ctrl Pts',(-0.792391461327318,-0.734615936171903,
1.2883190755065));
#19631=CARTESIAN_POINT('Ctrl Pts',(-0.806882581321256,-0.718338595112193,
1.288319084765));
#19632=CARTESIAN_POINT('Ctrl Pts',(-0.821284350360119,-0.70216161868754,
1.28831909396641));
#19633=CARTESIAN_POINT('Ctrl Pts',(-0.835451517519998,-0.685790724894018,
1.28797193184368));
#19634=CARTESIAN_POINT('Ctrl Pts',(-0.849391336665505,-0.669228599956957,
1.28727233489076));
#19635=CARTESIAN_POINT('Origin',(0.,0.,1.37171309575435));
#19636=CARTESIAN_POINT('',(-1.08521613661244,-0.642908916934714,1.10727038327973));
#19637=CARTESIAN_POINT('Ctrl Pts',(-1.81394816223928,-0.428377445609996,
1.63615580822897));
#19638=CARTESIAN_POINT('Ctrl Pts',(-1.75466459467969,-0.490704884304682,
1.59808263051822));
#19639=CARTESIAN_POINT('Ctrl Pts',(-1.68908545531116,-0.54441546832001,
1.55687869031203));
#19640=CARTESIAN_POINT('Ctrl Pts',(-1.52960471530763,-0.636822561166696,
1.4528510278119));
#19641=CARTESIAN_POINT('Ctrl Pts',(-1.43800725813254,-0.665855105856971,
1.3904370872311));
#19642=CARTESIAN_POINT('Ctrl Pts',(-1.2542115325179,-0.681216094986277,
1.25222975809873));
#19643=CARTESIAN_POINT('Ctrl Pts',(-1.16714103226326,-0.668566409010631,
1.18062438818012));
#19644=CARTESIAN_POINT('Ctrl Pts',(-1.08521613661244,-0.642908916934714,
1.10727038327973));
#19645=CARTESIAN_POINT('Origin',(0.,0.,1.10727038327973));
#19646=CARTESIAN_POINT('Ctrl Pts',(-1.01098164380599,-0.373486051296586,
1.28318517918604));
#19647=CARTESIAN_POINT('Ctrl Pts',(-1.23747555342208,-0.40602191942841,
1.537509268581));
#19648=CARTESIAN_POINT('Ctrl Pts',(-1.43047014156898,-0.30446532726343,
1.74606924121326));
#19649=CARTESIAN_POINT('Ctrl Pts',(-1.58996540824668,-0.0688162748016467,
1.90886509708284));
#19650=CARTESIAN_POINT('Ctrl Pts',(-1.02423814947078,-0.379996173302724,
1.26846828789983));
#19651=CARTESIAN_POINT('Ctrl Pts',(-1.25379621584498,-0.413260018127925,
1.51986220127974));
#19652=CARTESIAN_POINT('Ctrl Pts',(-1.4495127653333,-0.310691453231357,
1.72609931925976));
#19653=CARTESIAN_POINT('Ctrl Pts',(-1.61148865224617,-0.0719956513773679,
1.88702478432129));
#19654=CARTESIAN_POINT('Ctrl Pts',(-1.05021098685512,-0.388981181049685,
1.24114793592827));
#19655=CARTESIAN_POINT('Ctrl Pts',(-1.28554831174898,-0.422993564147046,
1.48712868773117));
#19656=CARTESIAN_POINT('Ctrl Pts',(-1.48619594640544,-0.317635541875723,
1.68884366634831));
#19657=CARTESIAN_POINT('Ctrl Pts',(-1.65214688300285,-0.0729037034540686,
1.84629652534568));
#19658=CARTESIAN_POINT('Ctrl Pts',(-1.11570416593891,-0.390726670926085,
1.18065052582665));
#19659=CARTESIAN_POINT('Ctrl Pts',(-1.36485769647198,-0.422167036078157,
1.41452066958594));
#19660=CARTESIAN_POINT('Ctrl Pts',(-1.57470193347746,-0.307195656373209,
1.60634085692189));
#19661=CARTESIAN_POINT('Ctrl Pts',(-1.74530108095234,-0.04566774902926,
1.75602521756878));
#19662=CARTESIAN_POINT('Ctrl Pts',(-1.1725125033894,-0.377231702026724,
1.13419834492991));
#19663=CARTESIAN_POINT('Ctrl Pts',(-1.43283860087532,-0.40328175100029,
1.35889748756925));
#19664=CARTESIAN_POINT('Ctrl Pts',(-1.64835039139676,-0.277966085037659,
1.54318426643096));
#19665=CARTESIAN_POINT('Ctrl Pts',(-1.81900536712132,-0.00100075866862149,
1.68700348817737));
#19666=CARTESIAN_POINT('Ctrl Pts',(-1.21448591285885,-0.362468171451202,
1.10179959977345));
#19667=CARTESIAN_POINT('Ctrl Pts',(-1.48279448162749,-0.383640993960513,
1.32012924726704));
#19668=CARTESIAN_POINT('Ctrl Pts',(-1.7017123916886,-0.249943984819037,
1.49916808705051));
#19669=CARTESIAN_POINT('Ctrl Pts',(-1.87123964304219,0.0386228559732266,
1.63891611912387));
#19670=CARTESIAN_POINT('',(-1.01462217612883,-0.373997862975653,1.28727233489076));
#19671=CARTESIAN_POINT('',(-1.20742290720348,-0.364905277844141,1.10727038327973));
#19672=CARTESIAN_POINT('Ctrl Pts',(-1.01462217612883,-0.373997862975653,
1.28727233489076));
#19673=CARTESIAN_POINT('Ctrl Pts',(-1.0440064014209,-0.388393237732341,
1.25472274024233));
#19674=CARTESIAN_POINT('Ctrl Pts',(-1.07127228109916,-0.391823670549174,
1.22803799031341));
#19675=CARTESIAN_POINT('Ctrl Pts',(-1.13395503796153,-0.386137988413888,
1.17079203987022));
#19676=CARTESIAN_POINT('Ctrl Pts',(-1.16846630960692,-0.378867340058898,
1.1405220316103));
#19677=CARTESIAN_POINT('Ctrl Pts',(-1.20742290720348,-0.364905277844141,
1.10727038327973));
#19678=CARTESIAN_POINT('Ctrl Pts',(-1.01462217612883,-0.373997862975653,
1.28727233489076));
#19679=CARTESIAN_POINT('Ctrl Pts',(-1.11493412912611,-0.387792676785358,
1.39987124007464));
#19680=CARTESIAN_POINT('Ctrl Pts',(-1.20865423507634,-0.375201374409042,
1.50346488650363));
#19681=CARTESIAN_POINT('Ctrl Pts',(-1.40394856048621,-0.287835131123856,
1.715480776583));
#19682=CARTESIAN_POINT('Ctrl Pts',(-1.50195515531182,-0.198779555753984,
1.81902921434248));
#19683=CARTESIAN_POINT('Ctrl Pts',(-1.58980227845634,-0.0690572297370878,
1.90869858745619));
#19684=CARTESIAN_POINT('Ctrl Pts',(-1.20742290720348,-0.364905277844141,
1.10727038327973));
#19685=CARTESIAN_POINT('Ctrl Pts',(-1.2881015973139,-0.372446289646659,
1.17697999301248));
#19686=CARTESIAN_POINT('Ctrl Pts',(-1.3704559615559,-0.364817298041905,
1.24430717677952));
#19687=CARTESIAN_POINT('Ctrl Pts',(-1.53992597283257,-0.308173273864792,
1.37795460947453));
#19688=CARTESIAN_POINT('Ctrl Pts',(-1.62124173855645,-0.257956459417358,
1.43952296396722));
#19689=CARTESIAN_POINT('Ctrl Pts',(-1.75990988600071,-0.127450637982168,
1.54779670475201));
#19690=CARTESIAN_POINT('Ctrl Pts',(-1.81609416413933,-0.0535283678677387,
1.59336495559369));
#19691=CARTESIAN_POINT('Ctrl Pts',(-1.86363850813291,0.0276890267571704,
1.63615580822897));
#19692=CARTESIAN_POINT('Ctrl Pts',(-1.08812850838495,-0.649602771712747,
1.10192461715937));
#19693=CARTESIAN_POINT('Ctrl Pts',(-1.34297974552473,-0.736092841324624,
1.32030517702043));
#19694=CARTESIAN_POINT('Ctrl Pts',(-1.58801866900221,-0.660305598163237,
1.49938098964776));
#19695=CARTESIAN_POINT('Ctrl Pts',(-1.82324527881738,-0.422241042228586,
1.63915205504133));
#19696=CARTESIAN_POINT('Ctrl Pts',(-1.07063084893098,-0.608736859462563,
1.13430265099724));
#19697=CARTESIAN_POINT('Ctrl Pts',(-1.32005612801352,-0.687616058553888,
1.35904945381843));
#19698=CARTESIAN_POINT('Ctrl Pts',(-1.55655247099159,-0.608897279480437,
1.54337045304296));
#19699=CARTESIAN_POINT('Ctrl Pts',(-1.78029541437304,-0.372779487140093,
1.68721036521565));
#19700=CARTESIAN_POINT('Ctrl Pts',(-1.04217626136028,-0.5578027141241,1.18072639205177));
#19701=CARTESIAN_POINT('Ctrl Pts',(-1.2834749683804,-0.627342551630417,
1.41463926643554));
#19702=CARTESIAN_POINT('Ctrl Pts',(-1.50849481334978,-0.546058002751383,
1.60649029622179));
#19703=CARTESIAN_POINT('Ctrl Pts',(-1.71737956252144,-0.313972100865309,
1.75619180366366));
#19704=CARTESIAN_POINT('Ctrl Pts',(-0.996637718803132,-0.510779237881579,
1.24117859886916));
#19705=CARTESIAN_POINT('Ctrl Pts',(-1.22630353645006,-0.572467001402757,
1.48719483570068));
#19706=CARTESIAN_POINT('Ctrl Pts',(-1.43804667102143,-0.491616133252193,
1.68893408523069));
#19707=CARTESIAN_POINT('Ctrl Pts',(-1.63186740528248,-0.26823580862317,
1.84639893874704));
#19708=CARTESIAN_POINT('Ctrl Pts',(-0.972472692862429,-0.497730252266281,
1.26847955290007));
#19709=CARTESIAN_POINT('Ctrl Pts',(-1.1965424430155,-0.55780480775003,1.51990601315848));
#19710=CARTESIAN_POINT('Ctrl Pts',(-1.40293468429945,-0.478797895551023,
1.72616419407532));
#19711=CARTESIAN_POINT('Ctrl Pts',(-1.59191672260126,-0.260780594211966,
1.88709951781477));
#19712=CARTESIAN_POINT('Ctrl Pts',(-0.958722904028868,-0.49236880332188,
1.28318566992362));
#19713=CARTESIAN_POINT('Ctrl Pts',(-1.17968618624264,-0.551916626543442,
1.53754047574671));
#19714=CARTESIAN_POINT('Ctrl Pts',(-1.38351688474614,-0.474283127502362,
1.74612008846831));
#19715=CARTESIAN_POINT('Ctrl Pts',(-1.57021499953936,-0.259468306198639,
1.90892450808845));
#19716=CARTESIAN_POINT('',(-0.962275025729455,-0.493314642657339,1.28727233489076));
#19717=CARTESIAN_POINT('Ctrl Pts',(-1.08521613661244,-0.642908916934714,
1.10727038327973));
#19718=CARTESIAN_POINT('Ctrl Pts',(-1.0754332329569,-0.618651911001871,
1.12805083925446));
#19719=CARTESIAN_POINT('Ctrl Pts',(-1.06308333609212,-0.593211674629724,
1.15131250789253));
#19720=CARTESIAN_POINT('Ctrl Pts',(-1.03791374180393,-0.554422984205748,
1.19194777349594));
#19721=CARTESIAN_POINT('Ctrl Pts',(-1.02533374006937,-0.537242802810029,
1.21108489280015));
#19722=CARTESIAN_POINT('Ctrl Pts',(-0.999433395982659,-0.512927734894534,
1.245266066507));
#19723=CARTESIAN_POINT('Ctrl Pts',(-0.98452570391201,-0.501969908730666,
1.26352342884102));
#19724=CARTESIAN_POINT('Ctrl Pts',(-0.962275025729455,-0.493314642657339,
1.28727233489076));
#19725=CARTESIAN_POINT('Ctrl Pts',(-0.962275025729455,-0.493314642657339,
1.28727233489076));
#19726=CARTESIAN_POINT('Ctrl Pts',(-1.06019965524839,-0.519074140629024,
1.39987124007464));
#19727=CARTESIAN_POINT('Ctrl Pts',(-1.15475382712427,-0.517846241724568,
1.50346488650363));
#19728=CARTESIAN_POINT('Ctrl Pts',(-1.35913828497575,-0.454602843714802,
1.715480776583));
#19729=CARTESIAN_POINT('Ctrl Pts',(-1.46714441944577,-0.377981286365636,
1.81902921434248));
#19730=CARTESIAN_POINT('Ctrl Pts',(-1.5699559447672,-0.259766273896473,
1.90869858745619));
#19731=CARTESIAN_POINT('Ctrl Pts',(-0.962275025729455,-0.493314642657339,
1.28727233489076));
#19732=CARTESIAN_POINT('Ctrl Pts',(-1.18245156164078,-0.551233034159898,
1.54044293163017));
#19733=CARTESIAN_POINT('Ctrl Pts',(-1.38558898119851,-0.472718500477254,
1.74808806329354));
#19734=CARTESIAN_POINT('Ctrl Pts',(-1.57168728440264,-0.257771041609407,
1.91020772988088));
#19735=CARTESIAN_POINT('Ctrl Pts',(-0.979724075862581,-0.453542382763444,
1.28727233489076));
#19736=CARTESIAN_POINT('Ctrl Pts',(-1.20168985388846,-0.502493528317088,
1.54044293163017));
#19737=CARTESIAN_POINT('Ctrl Pts',(-1.4011880115129,-0.416024993050259,
1.74808806329354));
#19738=CARTESIAN_POINT('Ctrl Pts',(-1.57821854873589,-0.194136776962957,
1.91020772988088));
#19739=CARTESIAN_POINT('Ctrl Pts',(-0.997173125995706,-0.413770122869549,
1.28727233489076));
#19740=CARTESIAN_POINT('Ctrl Pts',(-1.22092814613614,-0.453754022474278,
1.54044293163017));
#19741=CARTESIAN_POINT('Ctrl Pts',(-1.41678704182728,-0.359331485623264,
1.74808806329354));
#19742=CARTESIAN_POINT('Ctrl Pts',(-1.58474981306913,-0.130502512316506,
1.91020772988088));
#19743=CARTESIAN_POINT('Ctrl Pts',(-1.01462217612883,-0.373997862975653,
1.28727233489076));
#19744=CARTESIAN_POINT('Ctrl Pts',(-1.24016643838382,-0.405014516631467,
1.54044293163017));
#19745=CARTESIAN_POINT('Ctrl Pts',(-1.43238607214167,-0.302637978196268,
1.74808806329354));
#19746=CARTESIAN_POINT('Ctrl Pts',(-1.59128107740238,-0.0668682476700562,
1.91020772988088));
#19747=CARTESIAN_POINT('Ctrl Pts',(-0.962275025729455,-0.493314642657339,
1.28727233489076));
#19748=CARTESIAN_POINT('Ctrl Pts',(-0.971588210291795,-0.473624023308118,
1.28796759655004));
#19749=CARTESIAN_POINT('Ctrl Pts',(-0.980617871367769,-0.453798845322803,
1.2883190755065));
#19750=CARTESIAN_POINT('Ctrl Pts',(-0.989369770455727,-0.433840171694363,
1.288319084765));
#19751=CARTESIAN_POINT('Ctrl Pts',(-0.998067706113495,-0.414004561469673,
1.28831909396641));
#19752=CARTESIAN_POINT('Ctrl Pts',(-1.00648259836303,-0.394057020835215,
1.28797193184368));
#19753=CARTESIAN_POINT('Ctrl Pts',(-1.01462217612883,-0.373997862975653,
1.28727233489076));
#19754=CARTESIAN_POINT('Origin',(0.,0.,1.37171309575435));
#19755=CARTESIAN_POINT('',(-1.23077165948193,-0.27609248605185,1.10727038327973));
#19756=CARTESIAN_POINT('Ctrl Pts',(-1.85754313061971,0.153129647965883,
1.63615580822897));
#19757=CARTESIAN_POINT('Ctrl Pts',(-1.81335940151627,0.0607713534907818,
1.59083969670469));
#19758=CARTESIAN_POINT('Ctrl Pts',(-1.75708539039456,-0.0223614442500404,
1.54129005514746));
#19759=CARTESIAN_POINT('Ctrl Pts',(-1.61733286423933,-0.159600739735627,
1.42521036359321));
#19760=CARTESIAN_POINT('Ctrl Pts',(-1.53789592166465,-0.208550308549111,
1.36183966503053));
#19761=CARTESIAN_POINT('Ctrl Pts',(-1.37907079095174,-0.264206681902337,
1.23219371736399));
#19762=CARTESIAN_POINT('Ctrl Pts',(-1.30454791379682,-0.275306576910198,
1.17031259812848));
#19763=CARTESIAN_POINT('Ctrl Pts',(-1.23077165948193,-0.27609248605185,
1.10727038327973));
#19764=CARTESIAN_POINT('Origin',(0.,0.,1.10727038327973));
#19765=CARTESIAN_POINT('Ctrl Pts',(-1.07691421720911,-0.042795833893793,
1.28318517918604));
#19766=CARTESIAN_POINT('Ctrl Pts',(-1.30237686203014,-0.00374881610008784,
1.537509268581));
#19767=CARTESIAN_POINT('Ctrl Pts',(-1.45454290982716,0.152475850210932,
1.74606924121326));
#19768=CARTESIAN_POINT('Ctrl Pts',(-1.53341236060018,0.425878165039266,
1.90886509708284));
#19769=CARTESIAN_POINT('Ctrl Pts',(-1.091545040475,-0.0448924758011831,
1.26845681306972));
#19770=CARTESIAN_POINT('Ctrl Pts',(-1.32014932750452,-0.00559080476410112,
1.51984840181958));
#19771=CARTESIAN_POINT('Ctrl Pts',(-1.4745930125769,0.152438895007655,1.72608377212012));
#19772=CARTESIAN_POINT('Ctrl Pts',(-1.55488138991364,0.429508274607612,
1.88700775532559));
#19773=CARTESIAN_POINT('Ctrl Pts',(-1.11904054473513,-0.0454099470705951,
1.24111941924412));
#19774=CARTESIAN_POINT('Ctrl Pts',(-1.35337649424567,-0.00503268467650647,
1.48709402322589));
#19775=CARTESIAN_POINT('Ctrl Pts',(-1.51165038249935,0.15717562594847,1.68880469124906));
#19776=CARTESIAN_POINT('Ctrl Pts',(-1.59385438982847,0.441219201568136,
1.84625359892919));
#19777=CARTESIAN_POINT('Ctrl Pts',(-1.18191630764682,-0.0267999250011405,
1.1805768626608));
#19778=CARTESIAN_POINT('Ctrl Pts',(-1.42860644524989,0.0203022432084532,
1.41443159040039));
#19779=CARTESIAN_POINT('Ctrl Pts',(-1.59265822923791,0.194505783955957,
1.60624053738541));
#19780=CARTESIAN_POINT('Ctrl Pts',(-1.67408715628731,0.495974904441976,
1.7559150245411));
#19781=CARTESIAN_POINT('Ctrl Pts',(-1.23181557314521,0.0036323801669868,
1.1340877844534));
#19782=CARTESIAN_POINT('Ctrl Pts',(-1.48747160844964,0.059323221268054,
1.35876508657128));
#19783=CARTESIAN_POINT('Ctrl Pts',(-1.65371551508435,0.245130498049616,
1.54303391436826));
#19784=CARTESIAN_POINT('Ctrl Pts',(-1.73041945202573,0.561310568731046,
1.68683916414419));
#19785=CARTESIAN_POINT('Ctrl Pts',(-1.26719829440569,0.0306796703371001,
1.101666983688));
#19786=CARTESIAN_POINT('Ctrl Pts',(-1.52894260490194,0.0934843164788996,
1.31997051162989));
#19787=CARTESIAN_POINT('Ctrl Pts',(-1.69583409006838,0.288323673548526,
1.4989879457606));
#19788=CARTESIAN_POINT('Ctrl Pts',(-1.76787274990502,0.615197741545978,
1.63871928608013));
#19789=CARTESIAN_POINT('',(-1.08053472770428,-0.0421576093699569,1.28727233489076));
#19790=CARTESIAN_POINT('',(-1.22409607968053,1.1943445105165E-9,1.144533070421));
#19791=CARTESIAN_POINT('Ctrl Pts',(-1.08053472770428,-0.0421576093699569,
1.28727233489076));
#19792=CARTESIAN_POINT('Ctrl Pts',(-1.11292920208489,-0.0467681993550381,
1.25472274024224));
#19793=CARTESIAN_POINT('Ctrl Pts',(-1.13992065666394,-0.0416051146519816,
1.22803799031326));
#19794=CARTESIAN_POINT('Ctrl Pts',(-1.18752803009125,-0.0212174145555454,
1.18093412618539));
#19795=CARTESIAN_POINT('Ctrl Pts',(-1.20526565550415,-0.0119731083046825,
1.16336349462073));
#19796=CARTESIAN_POINT('Ctrl Pts',(-1.22409607968053,2.38868920650337E-9,
1.144533070421));
#19797=CARTESIAN_POINT('Ctrl Pts',(-1.08053472770428,-0.0421576093699569,
1.28727233489076));
#19798=CARTESIAN_POINT('Ctrl Pts',(-1.18019989616608,-0.0242791587196548,
1.39987124007464));
#19799=CARTESIAN_POINT('Ctrl Pts',(-1.26544208722232,0.0166569869072258,
1.50346488650363));
#19800=CARTESIAN_POINT('Ctrl Pts',(-1.42418037408903,0.160096487344471,
1.715480776583));
#19801=CARTESIAN_POINT('Ctrl Pts',(-1.48987049850469,0.275079075974333,
1.81902921434248));
#19802=CARTESIAN_POINT('Ctrl Pts',(-1.53333167412,0.425598593400271,1.90869858745619));
#19803=CARTESIAN_POINT('',(-1.26108935601086,0.0260686553993156,1.10727038327973));
#19804=CARTESIAN_POINT('Ctrl Pts',(-1.26108935601086,0.0260686553993152,
1.10727038327973));
#19805=CARTESIAN_POINT('Ctrl Pts',(-1.34014965076829,0.0438278133131024,
1.17697999301248));
#19806=CARTESIAN_POINT('Ctrl Pts',(-1.41611581747019,0.0765323136032917,
1.24430717677953));
#19807=CARTESIAN_POINT('Ctrl Pts',(-1.55978740991096,0.182773095427525,
1.37795460947454));
#19808=CARTESIAN_POINT('Ctrl Pts',(-1.62160544971256,0.255660077554636,
1.43952296396723));
#19809=CARTESIAN_POINT('Ctrl Pts',(-1.71055550747296,0.417882684528441,
1.54471868724288));
#19810=CARTESIAN_POINT('Ctrl Pts',(-1.74236185427976,0.503955443296111,
1.59041399531273));
#19811=CARTESIAN_POINT('Ctrl Pts',(-1.76386916735271,0.602229799711921,
1.63615580822897));
#19812=CARTESIAN_POINT('Ctrl Pts',(-1.22409607968053,2.38868920650337E-9,
1.144533070421));
#19813=CARTESIAN_POINT('Ctrl Pts',(-1.23602443718504,0.00758451261819888,
1.13260471290168));
#19814=CARTESIAN_POINT('Ctrl Pts',(-1.24839445491079,0.0162506540138241,
1.12016548273562));
#19815=CARTESIAN_POINT('Ctrl Pts',(-1.26108935601086,0.0260686553993153,
1.10727038327973));
#19816=CARTESIAN_POINT('Ctrl Pts',(-1.23578335387376,-0.281756991007075,
1.1017328493151));
#19817=CARTESIAN_POINT('Ctrl Pts',(-1.50493278576872,-0.285293785520307,
1.32007563441911));
#19818=CARTESIAN_POINT('Ctrl Pts',(-1.71461214828354,-0.137495264840182,
1.49912049044759));
#19819=CARTESIAN_POINT('Ctrl Pts',(-1.8648214414182,0.1616385710333,1.63886741740055));
#19820=CARTESIAN_POINT('Ctrl Pts',(-1.21381148288727,-0.256619313744399,
1.12604029619216));
#19821=CARTESIAN_POINT('Ctrl Pts',(-1.47730375097777,-0.255919204048238,
1.34917212439386));
#19822=CARTESIAN_POINT('Ctrl Pts',(-1.68029140190123,-0.108074844008926,
1.53213933043029));
#19823=CARTESIAN_POINT('Ctrl Pts',(-1.82267525691205,0.187017052056837,
1.67494641070563));
#19824=CARTESIAN_POINT('Ctrl Pts',(-1.17543855297398,-0.219711749650113,
1.16779612397806));
#19825=CARTESIAN_POINT('Ctrl Pts',(-1.42937433465483,-0.213070651520421,
1.39915507862237));
#19826=CARTESIAN_POINT('Ctrl Pts',(-1.62159457256361,-0.0660178837300448,
1.58891631513415));
#19827=CARTESIAN_POINT('Ctrl Pts',(-1.75213954537449,0.221600535375864,
1.73698522631427));
#19828=CARTESIAN_POINT('Ctrl Pts',(-1.11847368101377,-0.181934739915363,
1.22808906223352));
#19829=CARTESIAN_POINT('Ctrl Pts',(-1.35883455739468,-0.169938151077974,
1.47147297599238));
#19830=CARTESIAN_POINT('Ctrl Pts',(-1.53761229859012,-0.0262526925971351,
1.67105384595181));
#19831=CARTESIAN_POINT('Ctrl Pts',(-1.65481713073797,0.249117593166617,
1.82682748557708));
#19832=CARTESIAN_POINT('Ctrl Pts',(-1.08361696356336,-0.173143664137204,
1.26355539141207));
#19833=CARTESIAN_POINT('Ctrl Pts',(-1.31631931390947,-0.160806376565823,
1.51400180025811));
#19834=CARTESIAN_POINT('Ctrl Pts',(-1.48896648444242,-0.0212938283898121,
1.71948206324578));
#19835=CARTESIAN_POINT('Ctrl Pts',(-1.6016350942056,0.245739828560955,1.87979168962263));
#19836=CARTESIAN_POINT('Ctrl Pts',(-1.06394999292458,-0.172008888578299,
1.28318566992362));
#19837=CARTESIAN_POINT('Ctrl Pts',(-1.29249985168945,-0.160360824547434,
1.5375404757467));
#19838=CARTESIAN_POINT('Ctrl Pts',(-1.46236429518571,-0.0235398295887255,
1.74612008846831));
#19839=CARTESIAN_POINT('Ctrl Pts',(-1.57354332341336,0.238454096297827,
1.90892450808844));
#19840=CARTESIAN_POINT('',(-1.06762054184321,-0.171810769270086,1.28727233489076));
#19841=CARTESIAN_POINT('Ctrl Pts',(-1.23077165948193,-0.27609248605185,
1.10727038327973));
#19842=CARTESIAN_POINT('Ctrl Pts',(-1.21397173814619,-0.256045785977561,
1.1280508392544));
#19843=CARTESIAN_POINT('Ctrl Pts',(-1.19436482287745,-0.235667011409717,
1.15131250789248));
#19844=CARTESIAN_POINT('Ctrl Pts',(-1.15844075168685,-0.206554607000212,
1.19194777349561));
#19845=CARTESIAN_POINT('Ctrl Pts',(-1.14116749104443,-0.19410271785781,
1.21108489279989));
#19846=CARTESIAN_POINT('Ctrl Pts',(-1.10902103082118,-0.178981360555552,
1.24526606650677));
#19847=CARTESIAN_POINT('Ctrl Pts',(-1.09145681862839,-0.173166578774625,
1.26352342884084));
#19848=CARTESIAN_POINT('Ctrl Pts',(-1.06762054184321,-0.171810769270086,
1.28727233489076));
#19849=CARTESIAN_POINT('Ctrl Pts',(-1.06762054184321,-0.171810769270086,
1.28727233489076));
#19850=CARTESIAN_POINT('Ctrl Pts',(-1.16871252149279,-0.166049132983329,
1.39987124007464));
#19851=CARTESIAN_POINT('Ctrl Pts',(-1.25825944116939,-0.135662485730195,
1.50346488650363));
#19852=CARTESIAN_POINT('Ctrl Pts',(-1.43309732687145,-0.0123561690781437,
1.715480776583));
#19853=CARTESIAN_POINT('Ctrl Pts',(-1.51213990150266,0.0938909933754472,
1.81902921434248));
#19854=CARTESIAN_POINT('Ctrl Pts',(-1.57338902476662,0.238090659850088,
1.90869858745619));
#19855=CARTESIAN_POINT('Ctrl Pts',(-1.06762054184321,-0.171810769270086,
1.28727233489076));
#19856=CARTESIAN_POINT('Ctrl Pts',(-1.29491863831812,-0.158856141562724,
1.54044293163017));
#19857=CARTESIAN_POINT('Ctrl Pts',(-1.46385147967852,-0.0214114678431581,
1.74808806329354));
#19858=CARTESIAN_POINT('Ctrl Pts',(-1.5744190659244,0.240523251888612,1.91020772988088));
#19859=CARTESIAN_POINT('Ctrl Pts',(-1.07192527046357,-0.128593049303376,
1.28727233489076));
#19860=CARTESIAN_POINT('Ctrl Pts',(-1.2981540059198,-0.106557157682628,
1.54044293163017));
#19861=CARTESIAN_POINT('Ctrl Pts',(-1.46116778184124,0.0373276272898291,
1.74808806329354));
#19862=CARTESIAN_POINT('Ctrl Pts',(-1.56096659822788,0.303061305613997,
1.91020772988088));
#19863=CARTESIAN_POINT('Ctrl Pts',(-1.07622999908393,-0.0853753293366666,
1.28727233489076));
#19864=CARTESIAN_POINT('Ctrl Pts',(-1.30138937352148,-0.0542581738025321,
1.54044293163017));
#19865=CARTESIAN_POINT('Ctrl Pts',(-1.45848408400396,0.0960667224228176,
1.74808806329354));
#19866=CARTESIAN_POINT('Ctrl Pts',(-1.54751413053135,0.365599359339382,
1.91020772988088));
#19867=CARTESIAN_POINT('Ctrl Pts',(-1.08053472770428,-0.0421576093699569,
1.28727233489076));
#19868=CARTESIAN_POINT('Ctrl Pts',(-1.30462474112317,-0.00195918992243616,
1.54044293163017));
#19869=CARTESIAN_POINT('Ctrl Pts',(-1.45580038616668,0.154805817555805,
1.74808806329354));
#19870=CARTESIAN_POINT('Ctrl Pts',(-1.53406166283483,0.428137413064766,
1.91020772988088));
#19871=CARTESIAN_POINT('Ctrl Pts',(-1.06762054184321,-0.171810769270086,
1.28727233489076));
#19872=CARTESIAN_POINT('Ctrl Pts',(-1.0703931707,-0.150205945126616,1.28796759655004));
#19873=CARTESIAN_POINT('Ctrl Pts',(-1.07285457179227,-0.128560761691046,
1.2883190755065));
#19874=CARTESIAN_POINT('Ctrl Pts',(-1.07501055311346,-0.106874449528872,
1.288319084765));
#19875=CARTESIAN_POINT('Ctrl Pts',(-1.07715324084587,-0.0853218532357573,
1.28831909396641));
#19876=CARTESIAN_POINT('Ctrl Pts',(-1.07899214990169,-0.0637502700203498,
1.28797193184368));
#19877=CARTESIAN_POINT('Ctrl Pts',(-1.08053472770428,-0.0421576093699569,
1.28727233489076));
#19878=CARTESIAN_POINT('Origin',(0.,0.,1.37171309575435));
#19879=CARTESIAN_POINT('',(-1.25585067703094,0.117749801015232,1.10727038327973));
#19880=CARTESIAN_POINT('Ctrl Pts',(-1.71930883511106,0.719647344681869,
1.63615580822897));
#19881=CARTESIAN_POINT('Ctrl Pts',(-1.70798257074607,0.63437738084719,1.59808263051822));
#19882=CARTESIAN_POINT('Ctrl Pts',(-1.68649822169668,0.552378154622133,
1.55687869031203));
#19883=CARTESIAN_POINT('Ctrl Pts',(-1.61179111914083,0.383878819109613,
1.4528510278119));
#19884=CARTESIAN_POINT('Ctrl Pts',(-1.55475212125011,0.306551362590219,
1.3904370872311));
#19885=CARTESIAN_POINT('Ctrl Pts',(-1.41508721860523,0.186091644383524,
1.25222975809873));
#19886=CARTESIAN_POINT('Ctrl Pts',(-1.33721040532788,0.145146699351923,
1.18062438818012));
#19887=CARTESIAN_POINT('Ctrl Pts',(-1.25585067703094,0.117749801015232,
1.10727038327973));
#19888=CARTESIAN_POINT('Origin',(0.,0.,1.10727038327973));
#19889=CARTESIAN_POINT('Ctrl Pts',(-1.03743092372925,0.292083537906633,
1.28318517918604));
#19890=CARTESIAN_POINT('Ctrl Pts',(-1.23979244918951,0.39889124746765,1.537509268581));
#19891=CARTESIAN_POINT('Ctrl Pts',(-1.33623488367509,0.594491629104934,
1.74606924121327));
#19892=CARTESIAN_POINT('Ctrl Pts',(-1.32675822718598,0.878884682818485,
1.90886509708284));
#19893=CARTESIAN_POINT('Ctrl Pts',(-1.05199356151554,0.294610685989129,
1.26845681306972));
#19894=CARTESIAN_POINT('Ctrl Pts',(-1.25726427409018,0.402631406009325,
1.51984840181958));
#19895=CARTESIAN_POINT('Ctrl Pts',(-1.35531508433346,0.600652305106679,
1.72608377212012));
#19896=CARTESIAN_POINT('Ctrl Pts',(-1.34605472186502,0.88897141708892,1.88700775532559));
#19897=CARTESIAN_POINT('Ctrl Pts',(-1.07830248703538,0.302614092509142,
1.241120378339));
#19898=CARTESIAN_POINT('Ctrl Pts',(-1.28869195855349,0.413428941810946,
1.48709498232078));
#19899=CARTESIAN_POINT('Ctrl Pts',(-1.38909450341186,0.616606838701708,
1.68880599613843));
#19900=CARTESIAN_POINT('Ctrl Pts',(-1.3795008682383,0.912150767476994,1.84625490381856));
#19901=CARTESIAN_POINT('Ctrl Pts',(-1.13234954650475,0.339741650892322,
1.18057861631984));
#19902=CARTESIAN_POINT('Ctrl Pts',(-1.35241043892922,0.460769919763727,
1.41443334405943));
#19903=CARTESIAN_POINT('Ctrl Pts',(-1.4546018215964,0.67714071293772,1.6062429176887));
#19904=CARTESIAN_POINT('Ctrl Pts',(-1.4388862517722,0.989017806729704,1.7559174048444));
#19905=CARTESIAN_POINT('Ctrl Pts',(-1.17040376051197,0.384106544865058,
1.1340877844534));
#19906=CARTESIAN_POINT('Ctrl Pts',(-1.39633768248717,0.516073741815779,
1.35876508657128));
#19907=CARTESIAN_POINT('Ctrl Pts',(-1.49702742698245,0.744159155535353,
1.54303391436826));
#19908=CARTESIAN_POINT('Ctrl Pts',(-1.4722721909128,1.06856709212994,1.68683916414419));
#19909=CARTESIAN_POINT('Ctrl Pts',(-1.19569665581665,0.420763908606192,
1.101666983688));
#19910=CARTESIAN_POINT('Ctrl Pts',(-1.42522258493377,0.561378116697256,
1.31997051162989));
#19911=CARTESIAN_POINT('Ctrl Pts',(-1.52373714690789,0.798253662001989,
1.49898794576061));
#19912=CARTESIAN_POINT('Ctrl Pts',(-1.491240341739,1.13139054452039,1.63871928608014));
#19913=CARTESIAN_POINT('',(-1.04067701160391,0.293809324770207,1.28727233489076));
#19914=CARTESIAN_POINT('',(-1.19131159212569,0.414490807021284,1.10727038327973));
#19915=CARTESIAN_POINT('Ctrl Pts',(-1.04067701160391,0.293809324770207,
1.28727233489076));
#19916=CARTESIAN_POINT('Ctrl Pts',(-1.07291073821508,0.299434836228392,
1.25472274024218));
#19917=CARTESIAN_POINT('Ctrl Pts',(-1.0969856560603,0.312686039747429,1.22803799031299));
#19918=CARTESIAN_POINT('Ctrl Pts',(-1.14435511150582,0.354129853274474,
1.17079203987229));
#19919=CARTESIAN_POINT('Ctrl Pts',(-1.16800173688696,0.380297147864045,
1.14052203161246));
#19920=CARTESIAN_POINT('Ctrl Pts',(-1.19131159212569,0.414490807021284,
1.10727038327973));
#19921=CARTESIAN_POINT('Ctrl Pts',(-1.04067701160391,0.293809324770207,
1.28727233489076));
#19922=CARTESIAN_POINT('Ctrl Pts',(-1.12993947443311,0.341610972564374,
1.39987124007464));
#19923=CARTESIAN_POINT('Ctrl Pts',(-1.19835965101752,0.406884846288962,
1.50346488650363));
#19924=CARTESIAN_POINT('Ctrl Pts',(-1.30500348982786,0.592356746173702,
1.715480776583));
#19925=CARTESIAN_POINT('Ctrl Pts',(-1.33194693676576,0.722011051157661,
1.81902921434248));
#19926=CARTESIAN_POINT('Ctrl Pts',(-1.32676788217082,0.878593860895847,
1.90869858745619));
#19927=CARTESIAN_POINT('Ctrl Pts',(-1.19131159212569,0.414490807021284,
1.10727038327973));
#19928=CARTESIAN_POINT('Ctrl Pts',(-1.26101451903382,0.455811744539446,
1.17697999301248));
#19929=CARTESIAN_POINT('Ctrl Pts',(-1.32315639051141,0.510390409161015,
1.24430717677953));
#19930=CARTESIAN_POINT('Ctrl Pts',(-1.42696598762934,0.655828360684352,
1.37795460947454));
#19931=CARTESIAN_POINT('Ctrl Pts',(-1.46323512106126,0.744250824847066,
1.43952296396723));
#19932=CARTESIAN_POINT('Ctrl Pts',(-1.49770211069242,0.92602077179853,1.54471868724291));
#19933=CARTESIAN_POINT('Ctrl Pts',(-1.50135379887061,1.01770953159232,1.59041399531275));
#19934=CARTESIAN_POINT('Ctrl Pts',(-1.4914400228729,1.11782012388912,1.63615580822897));
#19935=CARTESIAN_POINT('Ctrl Pts',(-1.26214138440836,0.114046207919,1.10192461715937));
#19936=CARTESIAN_POINT('Ctrl Pts',(-1.51915795367952,0.193872070477571,
1.32030517702043));
#19937=CARTESIAN_POINT('Ctrl Pts',(-1.67285198321398,0.399215503609641,
1.49938098964775));
#19938=CARTESIAN_POINT('Ctrl Pts',(-1.72322347301172,0.730076507315209,
1.63915205504133));
#19939=CARTESIAN_POINT('Ctrl Pts',(-1.23350917110671,0.131128471412263,
1.12620814253777));
#19940=CARTESIAN_POINT('Ctrl Pts',(-1.48384440470434,0.213229856531406,
1.3493730700966));
#19941=CARTESIAN_POINT('Ctrl Pts',(-1.63116936194582,0.416549152036913,
1.53236753871639));
#19942=CARTESIAN_POINT('Ctrl Pts',(-1.67535851585319,0.741153963610053,
1.67519578767207));
#19943=CARTESIAN_POINT('Ctrl Pts',(-1.18566161414104,0.154321672329431,
1.16792358645355));
#19944=CARTESIAN_POINT('Ctrl Pts',(-1.42508536822678,0.239112514228605,
1.39930746388998));
#19945=CARTESIAN_POINT('Ctrl Pts',(-1.56242925297241,0.438352145622171,
1.58908978141842));
#19946=CARTESIAN_POINT('Ctrl Pts',(-1.59768412386215,0.752201465653604,
1.73717464481022));
#19947=CARTESIAN_POINT('Ctrl Pts',(-1.11989042845004,0.172598846101516,
1.2281493040678));
#19948=CARTESIAN_POINT('Ctrl Pts',(-1.34476711329973,0.258281860114562,
1.47154499595952));
#19949=CARTESIAN_POINT('Ctrl Pts',(-1.47038505632135,0.450170312236593,
1.67113613169255));
#19950=CARTESIAN_POINT('Ctrl Pts',(-1.49675459841166,0.748265815679372,
1.82691733765971));
#19951=CARTESIAN_POINT('Ctrl Pts',(-1.08406383481182,0.17018101435307,1.26357751389222));
#19952=CARTESIAN_POINT('Ctrl Pts',(-1.30156053800083,0.253820963688729,
1.51402822523202));
#19953=CARTESIAN_POINT('Ctrl Pts',(-1.42264323155934,0.439852505027486,
1.71951214242024));
#19954=CARTESIAN_POINT('Ctrl Pts',(-1.44728013834437,0.72862733638904,1.87982452105688));
#19955=CARTESIAN_POINT('Ctrl Pts',(-1.06503024353735,0.165188454635723,
1.28318566992362));
#19956=CARTESIAN_POINT('Ctrl Pts',(-1.27879462627691,0.246892212254839,
1.5375404757467));
#19957=CARTESIAN_POINT('Ctrl Pts',(-1.39806529952135,0.429507710856691,
1.74612008846831));
#19958=CARTESIAN_POINT('Ctrl Pts',(-1.42284226327066,0.713034950441279,
1.90892450808844));
#19959=CARTESIAN_POINT('',(-1.06845992077163,0.166511139289342,1.28727233489076));
#19960=CARTESIAN_POINT('Ctrl Pts',(-1.25585067703094,0.117749801015232,
1.10727038327973));
#19961=CARTESIAN_POINT('Ctrl Pts',(-1.23367823136702,0.13162388455433,1.12805083925461));
#19962=CARTESIAN_POINT('Ctrl Pts',(-1.20873355917026,0.144946380875815,
1.15131250789267));
#19963=CARTESIAN_POINT('Ctrl Pts',(-1.16557150946219,0.161532774289756,
1.1919477734965));
#19964=CARTESIAN_POINT('Ctrl Pts',(-1.1452958170136,0.168037493511785,1.21108489280069));
#19965=CARTESIAN_POINT('Ctrl Pts',(-1.11004996015928,0.172484956391182,
1.24526606650637));
#19966=CARTESIAN_POINT('Ctrl Pts',(-1.0915485353108,0.172587502434539,1.26352342884047));
#19967=CARTESIAN_POINT('Ctrl Pts',(-1.06845992077163,0.166511139289342,
1.28727233489076));
#19968=CARTESIAN_POINT('Ctrl Pts',(-1.06845992077163,0.166511139289342,
1.28727233489076));
#19969=CARTESIAN_POINT('Ctrl Pts',(-1.16282366323453,0.203229920731113,
1.39987124007464));
#19970=CARTESIAN_POINT('Ctrl Pts',(-1.23859785430383,0.259800859583567,
1.50346488650363));
#19971=CARTESIAN_POINT('Ctrl Pts',(-1.36677481743678,0.431100013478375,
1.715480776583));
#19972=CARTESIAN_POINT('Ctrl Pts',(-1.40911659430225,0.556572568507924,
1.81902921434248));
#19973=CARTESIAN_POINT('Ctrl Pts',(-1.42280782457595,0.712641620935351,
1.90869858745619));
#19974=CARTESIAN_POINT('Ctrl Pts',(-1.06845992077163,0.166511139289342,
1.28727233489076));
#19975=CARTESIAN_POINT('Ctrl Pts',(-1.28063005644821,0.24907069698643,1.54044293163017));
#19976=CARTESIAN_POINT('Ctrl Pts',(-1.3988219960746,0.431991468445894,1.74808806329354));
#19977=CARTESIAN_POINT('Ctrl Pts',(-1.42303573965083,0.715273453667736,
1.91020772988088));
#19978=CARTESIAN_POINT('Ctrl Pts',(-1.05919895104906,0.208943867782964,
1.28727233489076));
#19979=CARTESIAN_POINT('Ctrl Pts',(-1.26754579908091,0.29980976997318,1.54044293163017));
#19980=CARTESIAN_POINT('Ctrl Pts',(-1.37811826912839,0.487026359393917,
1.74808806329354));
#19981=CARTESIAN_POINT('Ctrl Pts',(-1.39091636119152,0.770593636045173,
1.91020772988088));
#19982=CARTESIAN_POINT('Ctrl Pts',(-1.04993798132648,0.251376596276585,
1.28727233489076));
#19983=CARTESIAN_POINT('Ctrl Pts',(-1.25446154171361,0.350548842959931,
1.54044293163017));
#19984=CARTESIAN_POINT('Ctrl Pts',(-1.35741454218218,0.542061250341939,
1.74808806329354));
#19985=CARTESIAN_POINT('Ctrl Pts',(-1.35879698273221,0.825913818422611,
1.91020772988088));
#19986=CARTESIAN_POINT('Ctrl Pts',(-1.04067701160391,0.293809324770207,
1.28727233489076));
#19987=CARTESIAN_POINT('Ctrl Pts',(-1.24137728434631,0.401287915946682,
1.54044293163017));
#19988=CARTESIAN_POINT('Ctrl Pts',(-1.33671081523597,0.597096141289962,
1.74808806329354));
#19989=CARTESIAN_POINT('Ctrl Pts',(-1.3266776042729,0.881234000800048,1.91020772988088));
#19990=CARTESIAN_POINT('Ctrl Pts',(-1.06845992077163,0.166511139289342,
1.28727233489076));
#19991=CARTESIAN_POINT('Ctrl Pts',(-1.06442058969234,0.187915337510244,
1.28796759655004));
#19992=CARTESIAN_POINT('Ctrl Pts',(-1.06007279171241,0.209261745030532,
1.2883190755065));
#19993=CARTESIAN_POINT('Ctrl Pts',(-1.05542181279351,0.230552888394581,
1.288319084765));
#19994=CARTESIAN_POINT('Ctrl Pts',(-1.05079951139632,0.251712752465176,
1.28831909396641));
#19995=CARTESIAN_POINT('Ctrl Pts',(-1.0458824320276,0.272796801398346,1.28797193184368));
#19996=CARTESIAN_POINT('Ctrl Pts',(-1.04067701160391,0.293809324770207,
1.28727233489076));
#19997=CARTESIAN_POINT('Origin',(0.,0.,1.37171309575435));
#19998=CARTESIAN_POINT('',(-1.15799828028598,0.500065917147839,1.10727038327973));
#19999=CARTESIAN_POINT('Ctrl Pts',(-1.4127766116927,1.21572094522251,1.63615580822897));
#20000=CARTESIAN_POINT('Ctrl Pts',(-1.42835456209775,1.13112438230172,1.59808263051822));
#20001=CARTESIAN_POINT('Ctrl Pts',(-1.4332608863651,1.04649945489987,1.55687869031203));
#20002=CARTESIAN_POINT('Ctrl Pts',(-1.41427936788009,0.863161299579019,
1.4528510278119));
#20003=CARTESIAN_POINT('Ctrl Pts',(-1.38392755544946,0.771992498477371,
1.3904370872311));
#20004=CARTESIAN_POINT('Ctrl Pts',(-1.2883224397548,0.614269670090823,1.25222975809873));
#20005=CARTESIAN_POINT('Ctrl Pts',(-1.22690987286759,0.551263454538706,
1.18062438818012));
#20006=CARTESIAN_POINT('Ctrl Pts',(-1.15799828028598,0.500065917147839,
1.10727038327973));
#20007=CARTESIAN_POINT('Origin',(0.,0.,1.10727038327973));
#20008=CARTESIAN_POINT('Ctrl Pts',(-0.896396663228496,0.598371737951084,
1.28318517918604));
#20009=CARTESIAN_POINT('Ctrl Pts',(-1.05584851328029,0.762485056494505,
1.53750926858099));
#20010=CARTESIAN_POINT('Ctrl Pts',(-1.08712687701302,0.978314425275392,
1.74606924121326));
#20011=CARTESIAN_POINT('Ctrl Pts',(-0.990231754426695,1.24585984429374,
1.90886509708283));
#20012=CARTESIAN_POINT('Ctrl Pts',(-0.909465623084801,0.605275301161475,
1.26845681306972));
#20013=CARTESIAN_POINT('Ctrl Pts',(-1.0713094336526,0.771441249464592,1.51984840181957));
#20014=CARTESIAN_POINT('Ctrl Pts',(-1.1033694726,0.990069682591155,1.72608377212011));
#20015=CARTESIAN_POINT('Ctrl Pts',(-1.00546683912554,1.26141584343747,1.88700775532558));
#20016=CARTESIAN_POINT('Ctrl Pts',(-0.932013737380385,0.621016981690704,
1.24112031232197));
#20017=CARTESIAN_POINT('Ctrl Pts',(-1.09786234356421,0.791422088358102,
1.48709491630373));
#20018=CARTESIAN_POINT('Ctrl Pts',(-1.13056538342229,1.01568188386468,1.68880590632087));
#20019=CARTESIAN_POINT('Ctrl Pts',(-1.03011319759962,1.29379626687142,1.84625481400099));
#20020=CARTESIAN_POINT('Ctrl Pts',(-0.971942506168049,0.673028944353635,
1.180578495595));
#20021=CARTESIAN_POINT('Ctrl Pts',(-1.14383306000902,0.856136223676182,
1.41443322333459));
#20022=CARTESIAN_POINT('Ctrl Pts',(-1.17416051125987,1.09349602729721,1.60624275382303));
#20023=CARTESIAN_POINT('Ctrl Pts',(-1.06283879403329,1.38525239147929,1.75591724097872));
#20024=CARTESIAN_POINT('Ctrl Pts',(-0.99442467311732,0.726981684724077,
1.1340877844534));
#20025=CARTESIAN_POINT('Ctrl Pts',(-1.16852049530615,0.92230736881738,1.35876508657127));
#20026=CARTESIAN_POINT('Ctrl Pts',(-1.19379986392409,1.17034433001556,1.54303391436824));
#20027=CARTESIAN_POINT('Ctrl Pts',(-1.0700086698298,1.47122482340641,1.68683916414417));
#20028=CARTESIAN_POINT('Ctrl Pts',(-1.00715189764781,0.769660843866381,
1.101666983688));
#20029=CARTESIAN_POINT('Ctrl Pts',(-1.18199184824263,0.974320315501956,
1.31997051162988));
#20030=CARTESIAN_POINT('Ctrl Pts',(-1.20248619530708,1.23004502025839,1.49898794576059));
#20031=CARTESIAN_POINT('Ctrl Pts',(-1.06863493884117,1.53683495813568,1.63871928608012));
#20032=CARTESIAN_POINT('',(-0.89895057878464,0.601016155111926,1.28727233489076));
#20033=CARTESIAN_POINT('',(-1.00491994924733,0.762339710524743,1.10727038327973));
#20034=CARTESIAN_POINT('Ctrl Pts',(-0.89895057878464,0.601016155111926,
1.28727233489076));
#20035=CARTESIAN_POINT('Ctrl Pts',(-0.927868295879635,0.616327103756397,
1.25472274024264));
#20036=CARTESIAN_POINT('Ctrl Pts',(-0.946670056292164,0.636369305963792,
1.22803799031384));
#20037=CARTESIAN_POINT('Ctrl Pts',(-0.978914242877163,0.690422681628326,
1.17079203987024));
#20038=CARTESIAN_POINT('Ctrl Pts',(-0.99331738130894,0.722616466765028,
1.14052203161));
#20039=CARTESIAN_POINT('Ctrl Pts',(-1.00491994924733,0.762339710524743,
1.10727038327973));
#20040=CARTESIAN_POINT('Ctrl Pts',(-0.89895057878464,0.601016155111926,
1.28727233489076));
#20041=CARTESIAN_POINT('Ctrl Pts',(-0.969072704191387,0.674061841710201,
1.39987124007464));
#20042=CARTESIAN_POINT('Ctrl Pts',(-1.01397342270847,0.757283981982513,
1.50346488650363));
#20043=CARTESIAN_POINT('Ctrl Pts',(-1.05808377148838,0.966632999495317,
1.715480776583));
#20044=CARTESIAN_POINT('Ctrl Pts',(-1.04364312863621,1.09826755410688,1.81902921434248));
#20045=CARTESIAN_POINT('Ctrl Pts',(-0.990330805779365,1.24558623976355,
1.90869858745619));
#20046=CARTESIAN_POINT('Ctrl Pts',(-1.00491994924733,0.762339710524743,
1.10727038327973));
#20047=CARTESIAN_POINT('Ctrl Pts',(-1.05844250017153,0.823177646383102,
1.17697999301248));
#20048=CARTESIAN_POINT('Ctrl Pts',(-1.10067719707672,0.894287935370973,
1.24430717677953));
#20049=CARTESIAN_POINT('Ctrl Pts',(-1.1544631922219,1.06468657657252,1.37795460947454));
#20050=CARTESIAN_POINT('Ctrl Pts',(-1.16163314380192,1.15998911590306,1.43952296396723));
#20051=CARTESIAN_POINT('Ctrl Pts',(-1.1382431962131,1.34351349395869,1.54471868724281));
#20052=CARTESIAN_POINT('Ctrl Pts',(-1.11338277308106,1.43184312013679,1.59041399531266));
#20053=CARTESIAN_POINT('Ctrl Pts',(-1.07301833748062,1.5239904260293,1.63615580822897));
#20054=CARTESIAN_POINT('Ctrl Pts',(-1.16512557173636,0.498487526286222,
1.10192461715937));
#20055=CARTESIAN_POINT('Ctrl Pts',(-1.38489530661629,0.653828920782168,
1.32030517702043));
#20056=CARTESIAN_POINT('Ctrl Pts',(-1.46761240439959,0.896616198000948,
1.49938098964775));
#20057=CARTESIAN_POINT('Ctrl Pts',(-1.41327686508626,1.22684935794256,1.63915205504132));
#20058=CARTESIAN_POINT('Ctrl Pts',(-1.13261600897808,0.505885883797787,
1.12620814253777));
#20059=CARTESIAN_POINT('Ctrl Pts',(-1.34532824088584,0.661326782584695,
1.3493730700966));
#20060=CARTESIAN_POINT('Ctrl Pts',(-1.4226134838877,0.900220838946926,1.53236753871639));
#20061=CARTESIAN_POINT('Ctrl Pts',(-1.3643314634289,1.22259355973874,1.67519578767207));
#20062=CARTESIAN_POINT('Ctrl Pts',(-1.07994282031224,0.513157335393552,
1.16792434557147));
#20063=CARTESIAN_POINT('Ctrl Pts',(-1.28144653067711,0.667784226973452,
1.39930822300789));
#20064=CARTESIAN_POINT('Ctrl Pts',(-1.35050022373305,0.899713500733371,
1.58909081893482));
#20065=CARTESIAN_POINT('Ctrl Pts',(-1.28704482486114,1.20909629592349,1.73717568232662));
#20066=CARTESIAN_POINT('Ctrl Pts',(-1.01174252544333,0.5102156806996,1.22815018770195));
#20067=CARTESIAN_POINT('Ctrl Pts',(-1.19913545447318,0.661195786769768,
1.47154587959366));
#20068=CARTESIAN_POINT('Ctrl Pts',(-1.25930861084253,0.882510125799203,
1.6711373385863));
#20069=CARTESIAN_POINT('Ctrl Pts',(-1.19227095916867,1.17416443346653,1.82691854455345));
#20070=CARTESIAN_POINT('Ctrl Pts',(-0.978417148622634,0.496845910594337,
1.26357751389222));
#20071=CARTESIAN_POINT('Ctrl Pts',(-1.15942263970987,0.643602406938538,
1.51402822523202));
#20072=CARTESIAN_POINT('Ctrl Pts',(-1.21709221666582,0.857945526599464,
1.71951214242024));
#20073=CARTESIAN_POINT('Ctrl Pts',(-1.15128697696661,1.14019993459331,1.87982452105687));
#20074=CARTESIAN_POINT('Ctrl Pts',(-0.961857913410637,0.486216000974361,
1.28318566992362));
#20075=CARTESIAN_POINT('Ctrl Pts',(-1.13991207295831,0.629977719122414,
1.5375404757467));
#20076=CARTESIAN_POINT('Ctrl Pts',(-1.19691393144611,0.840512044007264,
1.74612008846831));
#20077=CARTESIAN_POINT('Ctrl Pts',(-1.13286348887405,1.11781897562891,1.90892450808844));
#20078=CARTESIAN_POINT('',(-0.964710998256926,0.488533777383804,1.28727233489076));
#20079=CARTESIAN_POINT('Ctrl Pts',(-1.15799828028598,0.500065917147839,
1.10727038327973));
#20080=CARTESIAN_POINT('Ctrl Pts',(-1.13262370376054,0.50640929218822,1.12805083925429));
#20081=CARTESIAN_POINT('Ctrl Pts',(-1.10478303295006,0.511371411500259,
1.15131250789239));
#20082=CARTESIAN_POINT('Ctrl Pts',(-1.05860800687958,0.513808202166494,
1.19194777349505));
#20083=CARTESIAN_POINT('Ctrl Pts',(-1.03731460867033,0.513729024230272,
1.21108489279944));
#20084=CARTESIAN_POINT('Ctrl Pts',(-1.00241946522331,0.507067244033085,
1.24526606650681));
#20085=CARTESIAN_POINT('Ctrl Pts',(-0.984791876090385,0.501447516417348,
1.26352342884092));
#20086=CARTESIAN_POINT('Ctrl Pts',(-0.964710998256925,0.488533777383804,
1.28727233489076));
#20087=CARTESIAN_POINT('Ctrl Pts',(-0.964710998256925,0.488533777383804,
1.28727233489076));
#20088=CARTESIAN_POINT('Ctrl Pts',(-1.04310952295002,0.552615413818275,
1.39987124007464));
#20089=CARTESIAN_POINT('Ctrl Pts',(-1.09769367964031,0.629833086622262,
1.50346488650363));
#20090=CARTESIAN_POINT('Ctrl Pts',(-1.16666286599128,0.832357123065218,
1.715480776583));
#20091=CARTESIAN_POINT('Ctrl Pts',(-1.16815913695893,0.964772942765737,
1.81902921434248));
#20092=CARTESIAN_POINT('Ctrl Pts',(-1.13295228123076,1.11743425489732,1.90869858745619));
#20093=CARTESIAN_POINT('Ctrl Pts',(-0.964710998256926,0.488533777383804,
1.28727233489076));
#20094=CARTESIAN_POINT('Ctrl Pts',(-1.14098448197888,0.632616760336964,
1.54044293163017));
#20095=CARTESIAN_POINT('Ctrl Pts',(-1.19686606932897,0.843108069941918,
1.74808806329354));
#20096=CARTESIAN_POINT('Ctrl Pts',(-1.13235576030722,1.12000770619867,1.91020772988088));
#20097=CARTESIAN_POINT('Ctrl Pts',(-0.94279085843283,0.526027903293178,
1.28727233489076));
#20098=CARTESIAN_POINT('Ctrl Pts',(-1.11286137791709,0.676829228446517,
1.54044293163017));
#20099=CARTESIAN_POINT('Ctrl Pts',(-1.16016893831867,0.889051558128351,
1.74808806329354));
#20100=CARTESIAN_POINT('Ctrl Pts',(-1.08471353963759,1.16269489233868,1.91020772988088));
#20101=CARTESIAN_POINT('Ctrl Pts',(-0.920870718608735,0.563522029202552,
1.28727233489076));
#20102=CARTESIAN_POINT('Ctrl Pts',(-1.0847382738553,0.721041696556071,1.54044293163017));
#20103=CARTESIAN_POINT('Ctrl Pts',(-1.12347180730837,0.934995046314783,
1.74808806329354));
#20104=CARTESIAN_POINT('Ctrl Pts',(-1.03707131896797,1.20538207847869,1.91020772988088));
#20105=CARTESIAN_POINT('Ctrl Pts',(-0.89895057878464,0.601016155111926,
1.28727233489076));
#20106=CARTESIAN_POINT('Ctrl Pts',(-1.05661516979351,0.765254164665624,
1.54044293163017));
#20107=CARTESIAN_POINT('Ctrl Pts',(-1.08677467629807,0.980938534501216,
1.74808806329354));
#20108=CARTESIAN_POINT('Ctrl Pts',(-0.989429098298345,1.2480692646187,1.91020772988088));
#20109=CARTESIAN_POINT('Ctrl Pts',(-0.964710998256926,0.488533777383804,
1.28727233489076));
#20110=CARTESIAN_POINT('Ctrl Pts',(-0.954255105111255,0.507642157628472,
1.28796759655004));
#20111=CARTESIAN_POINT('Ctrl Pts',(-0.943523700818286,0.526600254136218,
1.2883190755065));
#20112=CARTESIAN_POINT('Ctrl Pts',(-0.932521031881151,0.545412103245543,
1.288319084765));
#20113=CARTESIAN_POINT('Ctrl Pts',(-0.921586204420601,0.564107960168957,
1.28831909396641));
#20114=CARTESIAN_POINT('Ctrl Pts',(-0.910394454615245,0.582640621209113,
1.28797193184368));
#20115=CARTESIAN_POINT('Ctrl Pts',(-0.89895057878464,0.601016155111926,
1.28727233489076));
#20116=CARTESIAN_POINT('Origin',(0.,0.,1.37171309575435));
#20117=CARTESIAN_POINT('',(-0.946792943618189,0.833432097145896,1.10727038327973));
#20118=CARTESIAN_POINT('Ctrl Pts',(-0.967951970128403,1.59279130921887,
1.63615580822897));
#20119=CARTESIAN_POINT('Ctrl Pts',(-1.00890925697988,1.51714904820957,1.59808263051822));
#20120=CARTESIAN_POINT('Ctrl Pts',(-1.03972598936032,1.43818209714157,1.55687869031203));
#20121=CARTESIAN_POINT('Ctrl Pts',(-1.07832809822747,1.25795153804723,1.4528510278119));
#20122=CARTESIAN_POINT('Ctrl Pts',(-1.07763451813115,1.16186562982554,1.3904370872311));
#20123=CARTESIAN_POINT('Ctrl Pts',(-1.03544768423092,0.982318700621183,
1.25222975809873));
#20124=CARTESIAN_POINT('Ctrl Pts',(-0.996510853667281,0.903418701916912,
1.18062438818013));
#20125=CARTESIAN_POINT('Ctrl Pts',(-0.946792943618189,0.833432097145896,
1.10727038327973));
#20126=CARTESIAN_POINT('Origin',(0.,0.,1.10727038327973));
#20127=CARTESIAN_POINT('Ctrl Pts',(-0.667616851768136,0.846087143183836,
1.28318517918604));
#20128=CARTESIAN_POINT('Ctrl Pts',(-0.768550768362021,1.05144151564591,
1.53750926858099));
#20129=CARTESIAN_POINT('Ctrl Pts',(-0.731603317170576,1.2663729891825,1.74606924121326));
#20130=CARTESIAN_POINT('Ctrl Pts',(-0.556774498193799,1.4908815637936,1.90886509708283));
#20131=CARTESIAN_POINT('Ctrl Pts',(-0.677912852846923,0.856691352655137,
1.26845681306972));
#20132=CARTESIAN_POINT('Ctrl Pts',(-0.780487361597375,1.06473704847503,
1.51984840181957));
#20133=CARTESIAN_POINT('Ctrl Pts',(-0.743418369261302,1.28257214132251,
1.72608377212011));
#20134=CARTESIAN_POINT('Ctrl Pts',(-0.566456856673053,1.5103840982294,1.88700775532558));
#20135=CARTESIAN_POINT('Ctrl Pts',(-0.694492950134685,0.878631748253103,
1.24111924840996));
#20136=CARTESIAN_POINT('Ctrl Pts',(-0.799566273875777,1.0919466731633,1.48709385239173));
#20137=CARTESIAN_POINT('Ctrl Pts',(-0.76136794175864,1.31533666464122,1.68880445881716));
#20138=CARTESIAN_POINT('Ctrl Pts',(-0.579890165126716,1.54879772833386,
1.84625336649728));
#20139=CARTESIAN_POINT('Ctrl Pts',(-0.716394511678363,0.940438249469778,
1.18057655035131));
#20140=CARTESIAN_POINT('Ctrl Pts',(-0.823288881893973,1.16770072295994,
1.41443127809089));
#20141=CARTESIAN_POINT('Ctrl Pts',(-0.778782224872494,1.4028158039603,1.60624011348192));
#20142=CARTESIAN_POINT('Ctrl Pts',(-0.582751305549681,1.64589229282024,
1.75591460063761));
#20143=CARTESIAN_POINT('Ctrl Pts',(-0.721104370153833,0.99869479210307,
1.13408778445339));
#20144=CARTESIAN_POINT('Ctrl Pts',(-0.826320380483541,1.23825912446584,
1.35876508657127));
#20145=CARTESIAN_POINT('Ctrl Pts',(-0.7737148524921,1.48196804720543,1.54303391436825));
#20146=CARTESIAN_POINT('Ctrl Pts',(-0.563005244955075,1.72986881834181,
1.68683916414417));
#20147=CARTESIAN_POINT('Ctrl Pts',(-0.720020094497306,1.0432180131865,1.101666983688));
#20148=CARTESIAN_POINT('Ctrl Pts',(-0.82305951402404,1.29188925333651,1.31997051162988));
#20149=CARTESIAN_POINT('Ctrl Pts',(-0.76352751669565,1.54143100170431,1.49898794576059));
#20150=CARTESIAN_POINT('Ctrl Pts',(-0.541424102512135,1.79184325828989,
1.63871928608012));
#20151=CARTESIAN_POINT('',(-0.669228599956957,0.849391336665505,1.28727233489076));
#20152=CARTESIAN_POINT('',(-0.720159740047643,1.03556549162895,1.10727038327973));
#20153=CARTESIAN_POINT('Ctrl Pts',(-0.669228599956957,0.849391336665505,
1.28727233489076));
#20154=CARTESIAN_POINT('Ctrl Pts',(-0.691999639905444,0.872888980165426,
1.25472274024256));
#20155=CARTESIAN_POINT('Ctrl Pts',(-0.7036877955768,0.897760310667323,1.22803799031376));
#20156=CARTESIAN_POINT('Ctrl Pts',(-0.717650427656563,0.959132127441791,
1.17079203987355));
#20157=CARTESIAN_POINT('Ctrl Pts',(-0.721400199597664,0.994201051127123,
1.14052203161356));
#20158=CARTESIAN_POINT('Ctrl Pts',(-0.720159740047643,1.03556549162895,
1.10727038327973));
#20159=CARTESIAN_POINT('Ctrl Pts',(-0.669228599956957,0.849391336665505,
1.28727233489076));
#20160=CARTESIAN_POINT('Ctrl Pts',(-0.713346345736856,0.940530841324424,
1.39987124007464));
#20161=CARTESIAN_POINT('Ctrl Pts',(-0.73033241101646,1.03355488521186,1.50346488650363));
#20162=CARTESIAN_POINT('Ctrl Pts',(-0.707591441492497,1.2462884798982,1.715480776583));
#20163=CARTESIAN_POINT('Ctrl Pts',(-0.653180259586497,1.36701797678012,
1.81902921434248));
#20164=CARTESIAN_POINT('Ctrl Pts',(-0.55695325007777,1.49065195897357,1.90869858745619));
#20165=CARTESIAN_POINT('Ctrl Pts',(-0.720159740047643,1.03556549162895,
1.10727038327973));
#20166=CARTESIAN_POINT('Ctrl Pts',(-0.752262754789917,1.10996518478287,
1.17697999301248));
#20167=CARTESIAN_POINT('Ctrl Pts',(-0.770456050723177,1.19064632759638,
1.24430717677952));
#20168=CARTESIAN_POINT('Ctrl Pts',(-0.768953495941758,1.36932585223818,
1.37795460947453));
#20169=CARTESIAN_POINT('Ctrl Pts',(-0.746322420853235,1.46217959017503,
1.43952296396722));
#20170=CARTESIAN_POINT('Ctrl Pts',(-0.667365107081823,1.62949375452132,
1.54471868724278));
#20171=CARTESIAN_POINT('Ctrl Pts',(-0.616426084068442,1.70581792784477,
1.59041399531263));
#20172=CARTESIAN_POINT('Ctrl Pts',(-0.549562141057365,1.78098192700405,
1.63615580822897));
#20173=CARTESIAN_POINT('Ctrl Pts',(-0.954059150195613,0.834133412413726,
1.10192461715937));
#20174=CARTESIAN_POINT('Ctrl Pts',(-1.11506945780848,1.04978444082665,1.32030517702044));
#20175=CARTESIAN_POINT('Ctrl Pts',(-1.11871269798568,1.30624985183955,1.49938098964776));
#20176=CARTESIAN_POINT('Ctrl Pts',(-0.96498887072721,1.60352964545243,1.63915205504134));
#20177=CARTESIAN_POINT('Ctrl Pts',(-0.920854500490905,0.831123661162971,
1.12620814253776));
#20178=CARTESIAN_POINT('Ctrl Pts',(-1.0751219753964,1.04468843542396,1.3493730700966));
#20179=CARTESIAN_POINT('Ctrl Pts',(-1.07480228609568,1.29577263793342,1.5323675387164));
#20180=CARTESIAN_POINT('Ctrl Pts',(-0.919754141507906,1.58435717993001,
1.67519578767208));
#20181=CARTESIAN_POINT('Ctrl Pts',(-0.868512346714968,0.821762669862001,
1.16792406090531));
#20182=CARTESIAN_POINT('Ctrl Pts',(-1.01237142622958,1.03108965362589,1.39930793834173));
#20183=CARTESIAN_POINT('Ctrl Pts',(-1.00637513236489,1.27300639515448,1.589090429871));
#20184=CARTESIAN_POINT('Ctrl Pts',(-0.850420920292679,1.5476381219134,1.73717529326279));
#20185=CARTESIAN_POINT('Ctrl Pts',(-0.80455912762015,0.797889917227132,
1.22814985715448));
#20186=CARTESIAN_POINT('Ctrl Pts',(-0.936124975293412,0.999388130632026,
1.4715455490462));
#20187=CARTESIAN_POINT('Ctrl Pts',(-0.924963031592627,1.22846526028813,
1.67113688711452));
#20188=CARTESIAN_POINT('Ctrl Pts',(-0.771080298579198,1.48512921647049,
1.82691809308168));
#20189=CARTESIAN_POINT('Ctrl Pts',(-0.776996174893135,0.774876067377614,
1.26357751389222));
#20190=CARTESIAN_POINT('Ctrl Pts',(-0.903792375271581,0.970383562355559,
1.51402822523203));
#20191=CARTESIAN_POINT('Ctrl Pts',(-0.892403735624943,1.19205686236992,
1.71951214242025));
#20192=CARTESIAN_POINT('Ctrl Pts',(-0.74259782479529,1.44016181895953,1.87982452105689));
#20193=CARTESIAN_POINT('Ctrl Pts',(-0.764532229061142,0.75964933747155,
1.28318566992362));
#20194=CARTESIAN_POINT('Ctrl Pts',(-0.889446983704125,0.951396617529428,
1.53754047574671));
#20195=CARTESIAN_POINT('Ctrl Pts',(-0.878600288371208,1.16924120209866,
1.74612008846832));
#20196=CARTESIAN_POINT('Ctrl Pts',(-0.73199214306239,1.41318309117925,1.90892450808845));
#20197=CARTESIAN_POINT('',(-0.766529441696069,0.762735325532963,1.28727233489076));
#20198=CARTESIAN_POINT('Ctrl Pts',(-0.946792943618189,0.833432097145897,
1.10727038327973));
#20199=CARTESIAN_POINT('Ctrl Pts',(-0.920700076575993,0.831623829941906,
1.12805083925451));
#20200=CARTESIAN_POINT('Ctrl Pts',(-0.892688645988233,0.827739845432993,
1.15131250789253));
#20201=CARTESIAN_POINT('Ctrl Pts',(-0.848020576826102,0.815788503303454,
1.19194777349529));
#20202=CARTESIAN_POINT('Ctrl Pts',(-0.827793819032997,0.809133178696536,
1.21108489279973));
#20203=CARTESIAN_POINT('Ctrl Pts',(-0.79666516876339,0.792014256883052,
1.24526606650818));
#20204=CARTESIAN_POINT('Ctrl Pts',(-0.781636926589457,0.78122235370212,
1.26352342884212));
#20205=CARTESIAN_POINT('Ctrl Pts',(-0.766529441696069,0.762735325532963,
1.28727233489076));
#20206=CARTESIAN_POINT('Ctrl Pts',(-0.766529441696069,0.762735325532963,
1.28727233489076));
#20207=CARTESIAN_POINT('Ctrl Pts',(-0.821288554787752,0.847907059902912,
1.39987124007464));
#20208=CARTESIAN_POINT('Ctrl Pts',(-0.849339599532016,0.938212862837218,
1.50346488650363));
#20209=CARTESIAN_POINT('Ctrl Pts',(-0.852349824604395,1.15213731807335,
1.715480776583));
#20210=CARTESIAN_POINT('Ctrl Pts',(-0.812854124246773,1.27853461941729,
1.81902921434248));
#20211=CARTESIAN_POINT('Ctrl Pts',(-0.732195474855993,1.41284463836769,
1.90869858745619));
#20212=CARTESIAN_POINT('Ctrl Pts',(-0.766529441696069,0.762735325532963,
1.28727233489076));
#20213=CARTESIAN_POINT('Ctrl Pts',(-0.889651396707116,0.954237887485567,
1.54044293163017));
#20214=CARTESIAN_POINT('Ctrl Pts',(-0.877752552661174,1.17169537927269,
1.74808806329354));
#20215=CARTESIAN_POINT('Ctrl Pts',(-0.730832909558243,1.41510780089433,
1.91020772988088));
#20216=CARTESIAN_POINT('Ctrl Pts',(-0.734095827783032,0.791620662577143,
1.28727233489076));
#20217=CARTESIAN_POINT('Ctrl Pts',(-0.849242331321591,0.987595926292982,
1.54044293163017));
#20218=CARTESIAN_POINT('Ctrl Pts',(-0.828654188454019,1.20405019596674,
1.74808806329354));
#20219=CARTESIAN_POINT('Ctrl Pts',(-0.672331399180314,1.44098347159841,
1.91020772988088));
#20220=CARTESIAN_POINT('Ctrl Pts',(-0.701662213869994,0.820505999621324,
1.28727233489076));
#20221=CARTESIAN_POINT('Ctrl Pts',(-0.808833265936067,1.0209539651004,1.54044293163017));
#20222=CARTESIAN_POINT('Ctrl Pts',(-0.779555824246864,1.23640501266079,
1.74808806329354));
#20223=CARTESIAN_POINT('Ctrl Pts',(-0.613829888802386,1.4668591423025,1.91020772988088));
#20224=CARTESIAN_POINT('Ctrl Pts',(-0.669228599956957,0.849391336665504,
1.28727233489076));
#20225=CARTESIAN_POINT('Ctrl Pts',(-0.768424200550542,1.05431200390781,
1.54044293163017));
#20226=CARTESIAN_POINT('Ctrl Pts',(-0.730457460039709,1.26875982935484,
1.74808806329354));
#20227=CARTESIAN_POINT('Ctrl Pts',(-0.555328378424457,1.49273481300659,
1.91020772988088));
#20228=CARTESIAN_POINT('Ctrl Pts',(-0.766529441696069,0.762735325532963,
1.28727233489076));
#20229=CARTESIAN_POINT('Ctrl Pts',(-0.750680482155644,0.777677426407089,
1.28796759655004));
#20230=CARTESIAN_POINT('Ctrl Pts',(-0.734615936171909,0.792391461327313,
1.2883190755065));
#20231=CARTESIAN_POINT('Ctrl Pts',(-0.718338595112193,0.806882581321256,
1.288319084765));
#20232=CARTESIAN_POINT('Ctrl Pts',(-0.702161618687529,0.82128435036013,
1.28831909396641));
#20233=CARTESIAN_POINT('Ctrl Pts',(-0.685790724893994,0.835451517520017,
1.28797193184368));
#20234=CARTESIAN_POINT('Ctrl Pts',(-0.669228599956957,0.849391336665505,
1.28727233489076));
#20235=CARTESIAN_POINT('Origin',(0.,0.,1.37171309575435));
#20236=CARTESIAN_POINT('',(-0.642908916934714,1.08521613661244,1.10727038327973));
#20237=CARTESIAN_POINT('Ctrl Pts',(-0.428377445609996,1.81394816223928,
1.63615580822897));
#20238=CARTESIAN_POINT('Ctrl Pts',(-0.490704884304683,1.75466459467969,
1.59808263051822));
#20239=CARTESIAN_POINT('Ctrl Pts',(-0.544415468320009,1.68908545531116,
1.55687869031203));
#20240=CARTESIAN_POINT('Ctrl Pts',(-0.636822561166696,1.52960471530763,
1.4528510278119));
#20241=CARTESIAN_POINT('Ctrl Pts',(-0.665855105856971,1.43800725813254,
1.3904370872311));
#20242=CARTESIAN_POINT('Ctrl Pts',(-0.681216094986278,1.2542115325179,1.25222975809873));
#20243=CARTESIAN_POINT('Ctrl Pts',(-0.66856640901063,1.16714103226325,1.18062438818012));
#20244=CARTESIAN_POINT('Ctrl Pts',(-0.642908916934714,1.08521613661244,
1.10727038327973));
#20245=CARTESIAN_POINT('Origin',(0.,0.,1.10727038327973));
#20246=CARTESIAN_POINT('Ctrl Pts',(-0.373486051296586,1.01098164380599,
1.28318517918604));
#20247=CARTESIAN_POINT('Ctrl Pts',(-0.40602191942841,1.23747555342209,1.537509268581));
#20248=CARTESIAN_POINT('Ctrl Pts',(-0.304465327263429,1.43047014156898,
1.74606924121326));
#20249=CARTESIAN_POINT('Ctrl Pts',(-0.0688162748016438,1.58996540824669,
1.90886509708284));
#20250=CARTESIAN_POINT('Ctrl Pts',(-0.382166213971436,1.02865698469238,
1.26356265747109));
#20251=CARTESIAN_POINT('Ctrl Pts',(-0.415747810278512,1.25921979945503,
1.51398032870897));
#20252=CARTESIAN_POINT('Ctrl Pts',(-0.312707553760736,1.45578649927555,
1.71944252353204));
#20253=CARTESIAN_POINT('Ctrl Pts',(-0.0730554435692729,1.61866306691267,
1.87974468006744));
#20254=CARTESIAN_POINT('Ctrl Pts',(-0.391657241669877,1.0633167753106,1.22810806352261));
#20255=CARTESIAN_POINT('Ctrl Pts',(-0.425647906592845,1.30153367691802,
1.4714667110343));
#20256=CARTESIAN_POINT('Ctrl Pts',(-0.318676377131988,1.50438827167773,
1.67103178775816));
#20257=CARTESIAN_POINT('Ctrl Pts',(-0.0707311879560992,1.67188067012364,
1.82679988540378));
#20258=CARTESIAN_POINT('Ctrl Pts',(-0.386793101125269,1.13146507111567,
1.16783895333641));
#20259=CARTESIAN_POINT('Ctrl Pts',(-0.416728995650738,1.38370624635607,
1.39917869757247));
#20260=CARTESIAN_POINT('Ctrl Pts',(-0.298796521842128,1.59505828371836,
1.58892894777221));
#20261=CARTESIAN_POINT('Ctrl Pts',(-0.0329933807603502,1.76565888855501,
1.73699566095833));
#20262=CARTESIAN_POINT('Ctrl Pts',(-0.373540819382843,1.18300585575676,
1.1260986586408));
#20263=CARTESIAN_POINT('Ctrl Pts',(-0.398429005793491,1.4453045731053,1.34921513358857));
#20264=CARTESIAN_POINT('Ctrl Pts',(-0.270901963247257,1.66164003747218,
1.53217466057836));
#20265=CARTESIAN_POINT('Ctrl Pts',(0.00890514499184177,1.83206393610154,
1.674981645914));
#20266=CARTESIAN_POINT('Ctrl Pts',(-0.362468171451202,1.21448591285885,
1.10179959977345));
#20267=CARTESIAN_POINT('Ctrl Pts',(-0.383640993960513,1.48279448162749,
1.32012924726704));
#20268=CARTESIAN_POINT('Ctrl Pts',(-0.249943984819036,1.7017123916886,1.49916808705051));
#20269=CARTESIAN_POINT('Ctrl Pts',(0.0386228559732295,1.87123964304219,
1.63891611912388));
#20270=CARTESIAN_POINT('',(-0.373997862975653,1.01462217612883,1.28727233489076));
#20271=CARTESIAN_POINT('',(-0.364905277844141,1.20742290720348,1.10727038327973));
#20272=CARTESIAN_POINT('Ctrl Pts',(-0.373997862975653,1.01462217612883,
1.28727233489076));
#20273=CARTESIAN_POINT('Ctrl Pts',(-0.388393237732322,1.04400640142086,
1.25472274024237));
#20274=CARTESIAN_POINT('Ctrl Pts',(-0.391823670549201,1.07127228109886,
1.22803799031368));
#20275=CARTESIAN_POINT('Ctrl Pts',(-0.386137988413871,1.13395503796173,
1.17079203987004));
#20276=CARTESIAN_POINT('Ctrl Pts',(-0.378867340058857,1.16846630960703,
1.1405220316102));
#20277=CARTESIAN_POINT('Ctrl Pts',(-0.364905277844141,1.20742290720348,
1.10727038327973));
#20278=CARTESIAN_POINT('Ctrl Pts',(-0.373997862975653,1.01462217612883,
1.28727233489076));
#20279=CARTESIAN_POINT('Ctrl Pts',(-0.387792676785359,1.11493412912611,
1.39987124007464));
#20280=CARTESIAN_POINT('Ctrl Pts',(-0.375201374409042,1.20865423507634,
1.50346488650363));
#20281=CARTESIAN_POINT('Ctrl Pts',(-0.287835131123856,1.40394856048621,
1.715480776583));
#20282=CARTESIAN_POINT('Ctrl Pts',(-0.198779555753984,1.50195515531182,
1.81902921434248));
#20283=CARTESIAN_POINT('Ctrl Pts',(-0.0690572297370878,1.58980227845634,
1.90869858745619));
#20284=CARTESIAN_POINT('Ctrl Pts',(-0.364905277844141,1.20742290720348,
1.10727038327973));
#20285=CARTESIAN_POINT('Ctrl Pts',(-0.372446289646659,1.2881015973139,1.17697999301248));
#20286=CARTESIAN_POINT('Ctrl Pts',(-0.364817298041905,1.3704559615559,1.24430717677952));
#20287=CARTESIAN_POINT('Ctrl Pts',(-0.308173273864789,1.53992597283257,
1.37795460947454));
#20288=CARTESIAN_POINT('Ctrl Pts',(-0.257956459417352,1.62124173855646,
1.43952296396723));
#20289=CARTESIAN_POINT('Ctrl Pts',(-0.127450637982162,1.75990988600072,
1.54779670475201));
#20290=CARTESIAN_POINT('Ctrl Pts',(-0.0535283678677282,1.81609416413934,
1.5933649555937));
#20291=CARTESIAN_POINT('Ctrl Pts',(0.0276890267571703,1.86363850813291,
1.63615580822897));
#20292=CARTESIAN_POINT('Ctrl Pts',(-0.649602771712747,1.08812850838495,
1.10192461715937));
#20293=CARTESIAN_POINT('Ctrl Pts',(-0.736092841324624,1.34297974552473,
1.32030517702043));
#20294=CARTESIAN_POINT('Ctrl Pts',(-0.660305598163237,1.58801866900221,
1.49938098964775));
#20295=CARTESIAN_POINT('Ctrl Pts',(-0.422241042228588,1.82324527881738,
1.63915205504133));
#20296=CARTESIAN_POINT('Ctrl Pts',(-0.618953337525111,1.07500526379448,
1.12620814253776));
#20297=CARTESIAN_POINT('Ctrl Pts',(-0.699675280139882,1.3257887054316,1.3493730700966));
#20298=CARTESIAN_POINT('Ctrl Pts',(-0.621781951952739,1.56448518294015,
1.5323675387164));
#20299=CARTESIAN_POINT('Ctrl Pts',(-0.385144875912219,1.79103288048413,
1.67519578767208));
#20300=CARTESIAN_POINT('Ctrl Pts',(-0.572065282586332,1.04992951600932,
1.16792267552995));
#20301=CARTESIAN_POINT('Ctrl Pts',(-0.644197802222636,1.29346620831953,
1.39930655296637));
#20302=CARTESIAN_POINT('Ctrl Pts',(-0.563737612015956,1.52169008642819,
1.58908853641612));
#20303=CARTESIAN_POINT('Ctrl Pts',(-0.330550471617962,1.73468787786897,
1.73717339980791));
#20304=CARTESIAN_POINT('Ctrl Pts',(-0.518619720423095,1.00746259753275,
1.22814823442989));
#20305=CARTESIAN_POINT('Ctrl Pts',(-0.581479904896343,1.23975486922368,
1.47154392632161));
#20306=CARTESIAN_POINT('Ctrl Pts',(-0.500074721257068,1.45417148278634,
1.67113467075223));
#20307=CARTESIAN_POINT('Ctrl Pts',(-0.274410020975489,1.65072103116966,
1.82691587671938));
#20308=CARTESIAN_POINT('Ctrl Pts',(-0.499517401914415,0.97705595580695,
1.26357751389222));
#20309=CARTESIAN_POINT('Ctrl Pts',(-0.559692616049941,1.20217681362938,
1.51402822523203));
#20310=CARTESIAN_POINT('Ctrl Pts',(-0.480360559198658,1.40948136690306,
1.71951214242025));
#20311=CARTESIAN_POINT('Ctrl Pts',(-0.261218023549743,1.59915063028856,
1.87982452105688));
#20312=CARTESIAN_POINT('Ctrl Pts',(-0.49236880332188,0.958722904028868,
1.28318566992362));
#20313=CARTESIAN_POINT('Ctrl Pts',(-0.551916626543442,1.17968618624264,
1.53754047574671));
#20314=CARTESIAN_POINT('Ctrl Pts',(-0.474283127502362,1.38351688474614,
1.74612008846831));
#20315=CARTESIAN_POINT('Ctrl Pts',(-0.25946830619864,1.57021499953936,1.90892450808845));
#20316=CARTESIAN_POINT('',(-0.493314642657339,0.962275025729455,1.28727233489076));
#20317=CARTESIAN_POINT('Ctrl Pts',(-0.642908916934714,1.08521613661244,
1.10727038327973));
#20318=CARTESIAN_POINT('Ctrl Pts',(-0.618651911001846,1.07543323295689,
1.12805083925448));
#20319=CARTESIAN_POINT('Ctrl Pts',(-0.59321167462972,1.06308333609212,1.15131250789253));
#20320=CARTESIAN_POINT('Ctrl Pts',(-0.554422984205854,1.037913741804,1.19194777349583));
#20321=CARTESIAN_POINT('Ctrl Pts',(-0.53724280281008,1.02533374006942,1.21108489280008));
#20322=CARTESIAN_POINT('Ctrl Pts',(-0.512927734894226,0.999433395982331,
1.24526606650743));
#20323=CARTESIAN_POINT('Ctrl Pts',(-0.501969908730524,0.984525703911643,
1.26352342884142));
#20324=CARTESIAN_POINT('Ctrl Pts',(-0.493314642657339,0.962275025729455,
1.28727233489076));
#20325=CARTESIAN_POINT('Ctrl Pts',(-0.493314642657339,0.962275025729455,
1.28727233489076));
#20326=CARTESIAN_POINT('Ctrl Pts',(-0.519074140629024,1.06019965524839,
1.39987124007464));
#20327=CARTESIAN_POINT('Ctrl Pts',(-0.517846241724568,1.15475382712427,
1.50346488650363));
#20328=CARTESIAN_POINT('Ctrl Pts',(-0.454602843714802,1.35913828497575,
1.715480776583));
#20329=CARTESIAN_POINT('Ctrl Pts',(-0.377981286365636,1.46714441944577,
1.81902921434248));
#20330=CARTESIAN_POINT('Ctrl Pts',(-0.259766273896473,1.5699559447672,1.90869858745619));
#20331=CARTESIAN_POINT('Ctrl Pts',(-0.493314642657339,0.962275025729455,
1.28727233489076));
#20332=CARTESIAN_POINT('Ctrl Pts',(-0.551233034159898,1.18245156164078,
1.54044293163017));
#20333=CARTESIAN_POINT('Ctrl Pts',(-0.472718500477254,1.38558898119851,
1.74808806329354));
#20334=CARTESIAN_POINT('Ctrl Pts',(-0.257771041609407,1.57168728440264,
1.91020772988088));
#20335=CARTESIAN_POINT('Ctrl Pts',(-0.453542382763444,0.979724075862581,
1.28727233489076));
#20336=CARTESIAN_POINT('Ctrl Pts',(-0.502493528317088,1.20168985388846,
1.54044293163017));
#20337=CARTESIAN_POINT('Ctrl Pts',(-0.416024993050259,1.4011880115129,1.74808806329354));
#20338=CARTESIAN_POINT('Ctrl Pts',(-0.194136776962956,1.57821854873589,
1.91020772988088));
#20339=CARTESIAN_POINT('Ctrl Pts',(-0.413770122869549,0.997173125995706,
1.28727233489076));
#20340=CARTESIAN_POINT('Ctrl Pts',(-0.453754022474278,1.22092814613614,
1.54044293163017));
#20341=CARTESIAN_POINT('Ctrl Pts',(-0.359331485623263,1.41678704182728,
1.74808806329354));
#20342=CARTESIAN_POINT('Ctrl Pts',(-0.130502512316506,1.58474981306913,
1.91020772988088));
#20343=CARTESIAN_POINT('Ctrl Pts',(-0.373997862975653,1.01462217612883,
1.28727233489076));
#20344=CARTESIAN_POINT('Ctrl Pts',(-0.405014516631467,1.24016643838382,
1.54044293163017));
#20345=CARTESIAN_POINT('Ctrl Pts',(-0.302637978196268,1.43238607214167,
1.74808806329354));
#20346=CARTESIAN_POINT('Ctrl Pts',(-0.066868247670056,1.59128107740238,
1.91020772988088));
#20347=CARTESIAN_POINT('Ctrl Pts',(-0.493314642657339,0.962275025729455,
1.28727233489076));
#20348=CARTESIAN_POINT('Ctrl Pts',(-0.473624023308118,0.971588210291795,
1.28796759655004));
#20349=CARTESIAN_POINT('Ctrl Pts',(-0.453798845322803,0.980617871367769,
1.2883190755065));
#20350=CARTESIAN_POINT('Ctrl Pts',(-0.433840171694363,0.989369770455727,
1.288319084765));
#20351=CARTESIAN_POINT('Ctrl Pts',(-0.414004561469676,0.998067706113494,
1.28831909396641));
#20352=CARTESIAN_POINT('Ctrl Pts',(-0.394057020835222,1.00648259836303,
1.28797193184368));
#20353=CARTESIAN_POINT('Ctrl Pts',(-0.373997862975653,1.01462217612883,
1.28727233489076));
#20354=CARTESIAN_POINT('Origin',(0.,0.,1.37171309575435));
#20355=CARTESIAN_POINT('',(-0.27609248605185,1.23077165948193,1.10727038327973));
#20356=CARTESIAN_POINT('Ctrl Pts',(0.153129647965883,1.85754313061971,1.63615580822897));
#20357=CARTESIAN_POINT('Ctrl Pts',(0.0607713534907839,1.81335940151627,
1.59083969670469));
#20358=CARTESIAN_POINT('Ctrl Pts',(-0.0223614442500398,1.75708539039456,
1.54129005514746));
#20359=CARTESIAN_POINT('Ctrl Pts',(-0.159600739735625,1.61733286423933,
1.42521036359322));
#20360=CARTESIAN_POINT('Ctrl Pts',(-0.208550308549109,1.53789592166466,
1.36183966503053));
#20361=CARTESIAN_POINT('Ctrl Pts',(-0.264206681902338,1.37907079095174,
1.23219371736399));
#20362=CARTESIAN_POINT('Ctrl Pts',(-0.275306576910198,1.30454791379682,
1.17031259812848));
#20363=CARTESIAN_POINT('Ctrl Pts',(-0.27609248605185,1.23077165948193,1.10727038327973));
#20364=CARTESIAN_POINT('Origin',(0.,0.,1.10727038327973));
#20365=CARTESIAN_POINT('Ctrl Pts',(-0.042795833893793,1.07691421720911,
1.28318517918604));
#20366=CARTESIAN_POINT('Ctrl Pts',(-0.00374881610008838,1.30237686203014,
1.53750926858099));
#20367=CARTESIAN_POINT('Ctrl Pts',(0.152475850210928,1.45454290982716,1.74606924121326));
#20368=CARTESIAN_POINT('Ctrl Pts',(0.425878165039256,1.53341236060018,1.90886509708283));
#20369=CARTESIAN_POINT('Ctrl Pts',(-0.0448924758011831,1.091545040475,1.26845681306972));
#20370=CARTESIAN_POINT('Ctrl Pts',(-0.00559080476410172,1.32014932750452,
1.51984840181958));
#20371=CARTESIAN_POINT('Ctrl Pts',(0.152438895007651,1.4745930125769,1.72608377212011));
#20372=CARTESIAN_POINT('Ctrl Pts',(0.429508274607602,1.55488138991364,1.88700775532559));
#20373=CARTESIAN_POINT('Ctrl Pts',(-0.0454099470705956,1.11904054473513,
1.24111941924413));
#20374=CARTESIAN_POINT('Ctrl Pts',(-0.00503268467650735,1.35337649424566,
1.4870940232259));
#20375=CARTESIAN_POINT('Ctrl Pts',(0.157175625948464,1.51165038249934,1.68880469124906));
#20376=CARTESIAN_POINT('Ctrl Pts',(0.441219201568124,1.59385438982847,1.84625359892919));
#20377=CARTESIAN_POINT('Ctrl Pts',(-0.026799925001142,1.18191630764682,
1.1805768626608));
#20378=CARTESIAN_POINT('Ctrl Pts',(0.0203022432084504,1.42860644524987,
1.41443159040039));
#20379=CARTESIAN_POINT('Ctrl Pts',(0.19450578395595,1.5926582292379,1.60624053738542));
#20380=CARTESIAN_POINT('Ctrl Pts',(0.49597490444196,1.6740871562873,1.75591502454111));
#20381=CARTESIAN_POINT('Ctrl Pts',(0.00363238016698291,1.2318155731452,
1.13408778445341));
#20382=CARTESIAN_POINT('Ctrl Pts',(0.0593232212680486,1.48747160844963,
1.35876508657129));
#20383=CARTESIAN_POINT('Ctrl Pts',(0.245130498049602,1.65371551508434,1.54303391436826));
#20384=CARTESIAN_POINT('Ctrl Pts',(0.561310568731024,1.73041945202573,1.68683916414419));
#20385=CARTESIAN_POINT('Ctrl Pts',(0.0306796703370947,1.26719829440569,
1.10166698368801));
#20386=CARTESIAN_POINT('Ctrl Pts',(0.093484316478892,1.52894260490193,1.3199705116299));
#20387=CARTESIAN_POINT('Ctrl Pts',(0.288323673548512,1.69583409006837,1.4989879457606));
#20388=CARTESIAN_POINT('Ctrl Pts',(0.615197741545956,1.76787274990501,1.63871928608014));
#20389=CARTESIAN_POINT('',(-0.0421576093699569,1.08053472770428,1.28727233489076));
#20390=CARTESIAN_POINT('',(0.0260686553993152,1.26108935601086,1.10727038327973));
#20391=CARTESIAN_POINT('Ctrl Pts',(-0.0421576093699569,1.08053472770428,
1.28727233489076));
#20392=CARTESIAN_POINT('Ctrl Pts',(-0.0467681993550378,1.11292920208489,
1.25472274024224));
#20393=CARTESIAN_POINT('Ctrl Pts',(-0.0416051146519907,1.13992065666392,
1.22803799031329));
#20394=CARTESIAN_POINT('Ctrl Pts',(-0.0168276724833753,1.19777852863159,
1.1707920398713));
#20395=CARTESIAN_POINT('Ctrl Pts',(0.000751694447766439,1.22835394451364,
1.14052203161151));
#20396=CARTESIAN_POINT('Ctrl Pts',(0.0260686553993151,1.26108935601086,
1.10727038327973));
#20397=CARTESIAN_POINT('Ctrl Pts',(-0.0421576093699569,1.08053472770428,
1.28727233489076));
#20398=CARTESIAN_POINT('Ctrl Pts',(-0.0242791587196549,1.18019989616608,
1.39987124007464));
#20399=CARTESIAN_POINT('Ctrl Pts',(0.0166569869072257,1.26544208722232,
1.50346488650363));
#20400=CARTESIAN_POINT('Ctrl Pts',(0.16009648734447,1.42418037408903,1.715480776583));
#20401=CARTESIAN_POINT('Ctrl Pts',(0.275079075974333,1.48987049850469,1.81902921434248));
#20402=CARTESIAN_POINT('Ctrl Pts',(0.425598593400272,1.53333167412,1.90869858745619));
#20403=CARTESIAN_POINT('Ctrl Pts',(0.0260686553993151,1.26108935601086,
1.10727038327973));
#20404=CARTESIAN_POINT('Ctrl Pts',(0.0438278133131022,1.34014965076829,
1.17697999301248));
#20405=CARTESIAN_POINT('Ctrl Pts',(0.0765323136032915,1.41611581747019,
1.24430717677953));
#20406=CARTESIAN_POINT('Ctrl Pts',(0.182773095427524,1.55978740991096,1.37795460947454));
#20407=CARTESIAN_POINT('Ctrl Pts',(0.255660077554632,1.62160544971256,1.43952296396723));
#20408=CARTESIAN_POINT('Ctrl Pts',(0.417882684528636,1.71055550747307,1.54471868724301));
#20409=CARTESIAN_POINT('Ctrl Pts',(0.503955443296384,1.74236185427982,1.59041399531286));
#20410=CARTESIAN_POINT('Ctrl Pts',(0.602229799711921,1.76386916735271,1.63615580822897));
#20411=CARTESIAN_POINT('Ctrl Pts',(-0.281756991007075,1.23578335387376,
1.1017328493151));
#20412=CARTESIAN_POINT('Ctrl Pts',(-0.285293785520307,1.50493278576873,
1.32007563441911));
#20413=CARTESIAN_POINT('Ctrl Pts',(-0.13749526484018,1.71461214828354,1.49912049044759));
#20414=CARTESIAN_POINT('Ctrl Pts',(0.161638571033305,1.8648214414182,1.63886741740056));
#20415=CARTESIAN_POINT('Ctrl Pts',(-0.248240087990173,1.20648752589178,
1.13414277848451));
#20416=CARTESIAN_POINT('Ctrl Pts',(-0.246204407588735,1.4681167114295,1.35885799576156));
#20417=CARTESIAN_POINT('Ctrl Pts',(-0.0982540365453086,1.66875380764494,
1.54315303441876));
#20418=CARTESIAN_POINT('Ctrl Pts',(0.195476545731356,1.80862652874333,1.68697274180731));
#20419=CARTESIAN_POINT('Ctrl Pts',(-0.208527189600699,1.16364558145094,
1.1806131496188));
#20420=CARTESIAN_POINT('Ctrl Pts',(-0.200108802601649,1.41464853624076,
1.41450373020722));
#20421=CARTESIAN_POINT('Ctrl Pts',(-0.0532621882672281,1.60356331755514,
1.60633610108347));
#20422=CARTESIAN_POINT('Ctrl Pts',(0.232035965773787,1.73053166984717,1.75602333097544));
#20423=CARTESIAN_POINT('Ctrl Pts',(-0.177813888094451,1.10574232216634,
1.24113368360637));
#20424=CARTESIAN_POINT('Ctrl Pts',(-0.165512243823413,1.34323970181786,
1.48714102989094));
#20425=CARTESIAN_POINT('Ctrl Pts',(-0.0231812731495988,1.5196432848029,
1.68887271819554));
#20426=CARTESIAN_POINT('Ctrl Pts',(0.249170413362428,1.63495516880573,1.84633185797669));
#20427=CARTESIAN_POINT('Ctrl Pts',(-0.172859970247478,1.07870022090367,
1.26846296103996));
#20428=CARTESIAN_POINT('Ctrl Pts',(-0.160752258036383,1.31037084404559,
1.51988605935312));
#20429=CARTESIAN_POINT('Ctrl Pts',(-0.0218314126094571,1.48224938444033,
1.72614171343829));
#20430=CARTESIAN_POINT('Ctrl Pts',(0.243918395495177,1.59461215150754,1.88707489423909));
#20431=CARTESIAN_POINT('Ctrl Pts',(-0.172008888578299,1.06394999292458,
1.28318566992362));
#20432=CARTESIAN_POINT('Ctrl Pts',(-0.160360824547434,1.29249985168946,
1.53754047574671));
#20433=CARTESIAN_POINT('Ctrl Pts',(-0.0235398295887241,1.46236429518571,
1.74612008846831));
#20434=CARTESIAN_POINT('Ctrl Pts',(0.238454096297831,1.57354332341336,1.90892450808845));
#20435=CARTESIAN_POINT('',(-0.171810769270086,1.06762054184321,1.28727233489076));
#20436=CARTESIAN_POINT('Ctrl Pts',(-0.27609248605185,1.23077165948193,1.10727038327973));
#20437=CARTESIAN_POINT('Ctrl Pts',(-0.256045785977569,1.21397173814619,
1.12805083925439));
#20438=CARTESIAN_POINT('Ctrl Pts',(-0.235667011409721,1.19436482287746,
1.15131250789247));
#20439=CARTESIAN_POINT('Ctrl Pts',(-0.206554607000384,1.15844075168706,
1.19194777349537));
#20440=CARTESIAN_POINT('Ctrl Pts',(-0.194102717857879,1.14116749104457,
1.21108489279973));
#20441=CARTESIAN_POINT('Ctrl Pts',(-0.178981360555473,1.10902103082101,
1.24526606650695));
#20442=CARTESIAN_POINT('Ctrl Pts',(-0.173166578774615,1.09145681862821,
1.26352342884102));
#20443=CARTESIAN_POINT('Ctrl Pts',(-0.171810769270086,1.06762054184321,
1.28727233489076));
#20444=CARTESIAN_POINT('Ctrl Pts',(-0.171810769270086,1.06762054184321,
1.28727233489076));
#20445=CARTESIAN_POINT('Ctrl Pts',(-0.166049132983329,1.16871252149279,
1.39987124007464));
#20446=CARTESIAN_POINT('Ctrl Pts',(-0.135662485730195,1.25825944116939,
1.50346488650363));
#20447=CARTESIAN_POINT('Ctrl Pts',(-0.0123561690781438,1.43309732687145,
1.715480776583));
#20448=CARTESIAN_POINT('Ctrl Pts',(0.0938909933754471,1.51213990150266,
1.81902921434248));
#20449=CARTESIAN_POINT('Ctrl Pts',(0.238090659850088,1.57338902476662,1.90869858745619));
#20450=CARTESIAN_POINT('Ctrl Pts',(-0.171810769270086,1.06762054184321,
1.28727233489076));
#20451=CARTESIAN_POINT('Ctrl Pts',(-0.158856141562724,1.29491863831812,
1.54044293163017));
#20452=CARTESIAN_POINT('Ctrl Pts',(-0.0214114678431582,1.46385147967851,
1.74808806329354));
#20453=CARTESIAN_POINT('Ctrl Pts',(0.240523251888612,1.5744190659244,1.91020772988088));
#20454=CARTESIAN_POINT('Ctrl Pts',(-0.128593049303376,1.07192527046357,
1.28727233489076));
#20455=CARTESIAN_POINT('Ctrl Pts',(-0.106557157682628,1.2981540059198,1.54044293163017));
#20456=CARTESIAN_POINT('Ctrl Pts',(0.0373276272898298,1.46116778184124,
1.74808806329354));
#20457=CARTESIAN_POINT('Ctrl Pts',(0.303061305613997,1.56096659822788,1.91020772988088));
#20458=CARTESIAN_POINT('Ctrl Pts',(-0.0853753293366666,1.07622999908393,
1.28727233489076));
#20459=CARTESIAN_POINT('Ctrl Pts',(-0.0542581738025321,1.30138937352148,
1.54044293163017));
#20460=CARTESIAN_POINT('Ctrl Pts',(0.0960667224228169,1.45848408400396,
1.74808806329354));
#20461=CARTESIAN_POINT('Ctrl Pts',(0.365599359339382,1.54751413053135,1.91020772988088));
#20462=CARTESIAN_POINT('Ctrl Pts',(-0.042157609369957,1.08053472770428,
1.28727233489076));
#20463=CARTESIAN_POINT('Ctrl Pts',(-0.00195918992243626,1.30462474112317,
1.54044293163017));
#20464=CARTESIAN_POINT('Ctrl Pts',(0.154805817555805,1.45580038616668,1.74808806329354));
#20465=CARTESIAN_POINT('Ctrl Pts',(0.428137413064766,1.53406166283483,1.91020772988088));
#20466=CARTESIAN_POINT('Ctrl Pts',(-0.171810769270086,1.06762054184321,
1.28727233489076));
#20467=CARTESIAN_POINT('Ctrl Pts',(-0.150205945126615,1.0703931707,1.28796759655004));
#20468=CARTESIAN_POINT('Ctrl Pts',(-0.128560761691045,1.07285457179227,
1.2883190755065));
#20469=CARTESIAN_POINT('Ctrl Pts',(-0.106874449528872,1.07501055311346,
1.288319084765));
#20470=CARTESIAN_POINT('Ctrl Pts',(-0.0853218532357455,1.07715324084587,
1.28831909396641));
#20471=CARTESIAN_POINT('Ctrl Pts',(-0.0637502700203263,1.07899214990169,
1.28797193184368));
#20472=CARTESIAN_POINT('Ctrl Pts',(-0.042157609369957,1.08053472770428,
1.28727233489076));
#20473=CARTESIAN_POINT('Origin',(0.,0.,1.37171309575435));
#20474=CARTESIAN_POINT('',(0.117749801015232,1.25585067703094,1.10727038327973));
#20475=CARTESIAN_POINT('Ctrl Pts',(0.719647344681868,1.71930883511106,1.63615580822897));
#20476=CARTESIAN_POINT('Ctrl Pts',(0.634377380847188,1.70798257074607,1.59808263051822));
#20477=CARTESIAN_POINT('Ctrl Pts',(0.552378154622132,1.68649822169668,1.55687869031203));
#20478=CARTESIAN_POINT('Ctrl Pts',(0.383878819109615,1.61179111914083,1.4528510278119));
#20479=CARTESIAN_POINT('Ctrl Pts',(0.306551362590222,1.55475212125012,1.3904370872311));
#20480=CARTESIAN_POINT('Ctrl Pts',(0.186091644383526,1.41508721860523,1.25222975809873));
#20481=CARTESIAN_POINT('Ctrl Pts',(0.145146699351924,1.33721040532788,1.18062438818012));
#20482=CARTESIAN_POINT('Ctrl Pts',(0.117749801015232,1.25585067703094,1.10727038327973));
#20483=CARTESIAN_POINT('Origin',(0.,0.,1.10727038327973));
#20484=CARTESIAN_POINT('Ctrl Pts',(0.292083537906633,1.03743092372925,1.28318517918604));
#20485=CARTESIAN_POINT('Ctrl Pts',(0.398891247467645,1.23979244918951,1.53750926858099));
#20486=CARTESIAN_POINT('Ctrl Pts',(0.594491629104918,1.33623488367508,1.74606924121325));
#20487=CARTESIAN_POINT('Ctrl Pts',(0.87888468281845,1.32675822718598,1.90886509708282));
#20488=CARTESIAN_POINT('Ctrl Pts',(0.294610685989129,1.05199356151554,1.26845681306972));
#20489=CARTESIAN_POINT('Ctrl Pts',(0.40263140600932,1.25726427409018,1.51984840181957));
#20490=CARTESIAN_POINT('Ctrl Pts',(0.600652305106663,1.35531508433345,1.7260837721201));
#20491=CARTESIAN_POINT('Ctrl Pts',(0.888971417088885,1.34605472186503,1.88700775532557));
#20492=CARTESIAN_POINT('Ctrl Pts',(0.302614092509143,1.07830248703539,1.241120378339));
#20493=CARTESIAN_POINT('Ctrl Pts',(0.413428941810942,1.28869195855348,1.48709498232076));
#20494=CARTESIAN_POINT('Ctrl Pts',(0.616606838701691,1.38909450341185,1.6888059961384));
#20495=CARTESIAN_POINT('Ctrl Pts',(0.912150767476957,1.3795008682383,1.84625490381853));
#20496=CARTESIAN_POINT('Ctrl Pts',(0.339741650892327,1.13234954650476,1.18057861631984));
#20497=CARTESIAN_POINT('Ctrl Pts',(0.460769919763728,1.35241043892922,1.41443334405942));
#20498=CARTESIAN_POINT('Ctrl Pts',(0.677140712937703,1.45460182159639,1.60624291768869));
#20499=CARTESIAN_POINT('Ctrl Pts',(0.989017806729666,1.43888625177221,1.75591740484438));
#20500=CARTESIAN_POINT('Ctrl Pts',(0.384106544865064,1.17040376051198,1.13408778445339));
#20501=CARTESIAN_POINT('Ctrl Pts',(0.516073741815779,1.39633768248717,1.35876508657127));
#20502=CARTESIAN_POINT('Ctrl Pts',(0.744159155535338,1.49702742698244,1.54303391436824));
#20503=CARTESIAN_POINT('Ctrl Pts',(1.06856709212991,1.47227219091281,1.68683916414416));
#20504=CARTESIAN_POINT('Ctrl Pts',(0.420763908606199,1.19569665581666,1.101666983688));
#20505=CARTESIAN_POINT('Ctrl Pts',(0.56137811669726,1.42522258493377,1.31997051162988));
#20506=CARTESIAN_POINT('Ctrl Pts',(0.798253662001981,1.52373714690789,1.49898794576058));
#20507=CARTESIAN_POINT('Ctrl Pts',(1.13139054452036,1.49124034173901,1.63871928608011));
#20508=CARTESIAN_POINT('',(0.293809324770207,1.04067701160391,1.28727233489076));
#20509=CARTESIAN_POINT('',(0.414490807021284,1.19131159212569,1.10727038327973));
#20510=CARTESIAN_POINT('Ctrl Pts',(0.293809324770207,1.04067701160391,1.28727233489076));
#20511=CARTESIAN_POINT('Ctrl Pts',(0.299434836228389,1.07291073821506,1.2547227402422));
#20512=CARTESIAN_POINT('Ctrl Pts',(0.312686039747463,1.09698565606033,1.22803799031295));
#20513=CARTESIAN_POINT('Ctrl Pts',(0.354129853274083,1.14435511150538,1.17079203987282));
#20514=CARTESIAN_POINT('Ctrl Pts',(0.380297147863541,1.1680017368866,1.14052203161296));
#20515=CARTESIAN_POINT('Ctrl Pts',(0.414490807021284,1.19131159212569,1.10727038327973));
#20516=CARTESIAN_POINT('Ctrl Pts',(0.293809324770207,1.04067701160391,1.28727233489076));
#20517=CARTESIAN_POINT('Ctrl Pts',(0.341610972564374,1.12993947443311,1.39987124007464));
#20518=CARTESIAN_POINT('Ctrl Pts',(0.406884846288962,1.19835965101752,1.50346488650363));
#20519=CARTESIAN_POINT('Ctrl Pts',(0.592356746173702,1.30500348982786,1.715480776583));
#20520=CARTESIAN_POINT('Ctrl Pts',(0.722011051157661,1.33194693676576,1.81902921434248));
#20521=CARTESIAN_POINT('Ctrl Pts',(0.878593860895847,1.32676788217082,1.90869858745619));
#20522=CARTESIAN_POINT('Ctrl Pts',(0.414490807021284,1.19131159212569,1.10727038327973));
#20523=CARTESIAN_POINT('Ctrl Pts',(0.455811744539446,1.26101451903382,1.17697999301248));
#20524=CARTESIAN_POINT('Ctrl Pts',(0.510390409161015,1.32315639051141,1.24430717677953));
#20525=CARTESIAN_POINT('Ctrl Pts',(0.655828360684359,1.42696598762934,1.37795460947455));
#20526=CARTESIAN_POINT('Ctrl Pts',(0.744250824847078,1.46323512106126,1.43952296396724));
#20527=CARTESIAN_POINT('Ctrl Pts',(0.926020771798293,1.49770211069237,1.54471868724277));
#20528=CARTESIAN_POINT('Ctrl Pts',(1.01770953159202,1.50135379887064,1.59041399531261));
#20529=CARTESIAN_POINT('Ctrl Pts',(1.11782012388912,1.4914400228729,1.63615580822897));
#20530=CARTESIAN_POINT('Ctrl Pts',(0.114046207919,1.26214138440836,1.10192461715937));
#20531=CARTESIAN_POINT('Ctrl Pts',(0.193872070477572,1.51915795367953,1.32030517702043));
#20532=CARTESIAN_POINT('Ctrl Pts',(0.399215503609646,1.67285198321398,1.49938098964776));
#20533=CARTESIAN_POINT('Ctrl Pts',(0.730076507315222,1.72322347301172,1.63915205504133));
#20534=CARTESIAN_POINT('Ctrl Pts',(0.131128471412264,1.23350917110672,1.12620814253776));
#20535=CARTESIAN_POINT('Ctrl Pts',(0.213229856531408,1.48384440470435,1.3493730700966));
#20536=CARTESIAN_POINT('Ctrl Pts',(0.416549152036918,1.63116936194582,1.53236753871639));
#20537=CARTESIAN_POINT('Ctrl Pts',(0.741153963610066,1.67535851585319,1.67519578767207));
#20538=CARTESIAN_POINT('Ctrl Pts',(0.15432167232943,1.18566161414104,1.16792358645355));
#20539=CARTESIAN_POINT('Ctrl Pts',(0.239112514228604,1.42508536822678,1.39930746388997));
#20540=CARTESIAN_POINT('Ctrl Pts',(0.438352145622179,1.56242925297243,1.58908978141844));
#20541=CARTESIAN_POINT('Ctrl Pts',(0.752201465653619,1.59768412386216,1.73717464481024));
#20542=CARTESIAN_POINT('Ctrl Pts',(0.172598846101516,1.11989042845005,1.22814930406781));
#20543=CARTESIAN_POINT('Ctrl Pts',(0.258281860114563,1.34476711329974,1.47154499595953));
#20544=CARTESIAN_POINT('Ctrl Pts',(0.450170312236601,1.47038505632136,1.67113613169257));
#20545=CARTESIAN_POINT('Ctrl Pts',(0.748265815679387,1.49675459841166,1.82691733765972));
#20546=CARTESIAN_POINT('Ctrl Pts',(0.17018101435307,1.08406383481183,1.26357751389222));
#20547=CARTESIAN_POINT('Ctrl Pts',(0.25382096368873,1.30156053800084,1.51402822523203));
#20548=CARTESIAN_POINT('Ctrl Pts',(0.439852505027491,1.42264323155934,1.71951214242025));
#20549=CARTESIAN_POINT('Ctrl Pts',(0.728627336389052,1.44728013834437,1.87982452105688));
#20550=CARTESIAN_POINT('Ctrl Pts',(0.165188454635723,1.06503024353735,1.28318566992362));
#20551=CARTESIAN_POINT('Ctrl Pts',(0.24689221225484,1.27879462627691,1.53754047574671));
#20552=CARTESIAN_POINT('Ctrl Pts',(0.429507710856696,1.39806529952135,1.74612008846832));
#20553=CARTESIAN_POINT('Ctrl Pts',(0.71303495044129,1.42284226327066,1.90892450808845));
#20554=CARTESIAN_POINT('',(0.166511139289342,1.06845992077163,1.28727233489076));
#20555=CARTESIAN_POINT('Ctrl Pts',(0.117749801015232,1.25585067703094,1.10727038327973));
#20556=CARTESIAN_POINT('Ctrl Pts',(0.13162388455422,1.23367823136719,1.12805083925445));
#20557=CARTESIAN_POINT('Ctrl Pts',(0.144946380875765,1.2087335591704,1.15131250789254));
#20558=CARTESIAN_POINT('Ctrl Pts',(0.161532774289144,1.16557150946378,1.19194777349501));
#20559=CARTESIAN_POINT('Ctrl Pts',(0.168037493511643,1.1452958170147,1.21108489279962));
#20560=CARTESIAN_POINT('Ctrl Pts',(0.172484956391369,1.11004996015782,1.24526606650779));
#20561=CARTESIAN_POINT('Ctrl Pts',(0.172587502434193,1.09154853530949,1.26352342884182));
#20562=CARTESIAN_POINT('Ctrl Pts',(0.166511139289342,1.06845992077163,1.28727233489076));
#20563=CARTESIAN_POINT('Ctrl Pts',(0.166511139289342,1.06845992077163,1.28727233489076));
#20564=CARTESIAN_POINT('Ctrl Pts',(0.203229920731113,1.16282366323453,1.39987124007464));
#20565=CARTESIAN_POINT('Ctrl Pts',(0.259800859583567,1.23859785430383,1.50346488650363));
#20566=CARTESIAN_POINT('Ctrl Pts',(0.431100013478375,1.36677481743678,1.715480776583));
#20567=CARTESIAN_POINT('Ctrl Pts',(0.556572568507924,1.40911659430225,1.81902921434248));
#20568=CARTESIAN_POINT('Ctrl Pts',(0.712641620935351,1.42280782457595,1.90869858745619));
#20569=CARTESIAN_POINT('Ctrl Pts',(0.166511139289342,1.06845992077163,1.28727233489076));
#20570=CARTESIAN_POINT('Ctrl Pts',(0.24907069698643,1.28063005644821,1.54044293163017));
#20571=CARTESIAN_POINT('Ctrl Pts',(0.431991468445894,1.3988219960746,1.74808806329354));
#20572=CARTESIAN_POINT('Ctrl Pts',(0.715273453667735,1.42303573965083,1.91020772988088));
#20573=CARTESIAN_POINT('Ctrl Pts',(0.208943867782964,1.05919895104906,1.28727233489076));
#20574=CARTESIAN_POINT('Ctrl Pts',(0.29980976997318,1.26754579908091,1.54044293163017));
#20575=CARTESIAN_POINT('Ctrl Pts',(0.487026359393917,1.37811826912839,1.74808806329354));
#20576=CARTESIAN_POINT('Ctrl Pts',(0.770593636045173,1.39091636119152,1.91020772988088));
#20577=CARTESIAN_POINT('Ctrl Pts',(0.251376596276585,1.04993798132648,1.28727233489076));
#20578=CARTESIAN_POINT('Ctrl Pts',(0.350548842959931,1.25446154171361,1.54044293163017));
#20579=CARTESIAN_POINT('Ctrl Pts',(0.542061250341939,1.35741454218218,1.74808806329354));
#20580=CARTESIAN_POINT('Ctrl Pts',(0.82591381842261,1.35879698273221,1.91020772988088));
#20581=CARTESIAN_POINT('Ctrl Pts',(0.293809324770207,1.04067701160391,1.28727233489076));
#20582=CARTESIAN_POINT('Ctrl Pts',(0.401287915946682,1.24137728434631,1.54044293163017));
#20583=CARTESIAN_POINT('Ctrl Pts',(0.597096141289962,1.33671081523597,1.74808806329354));
#20584=CARTESIAN_POINT('Ctrl Pts',(0.881234000800047,1.3266776042729,1.91020772988088));
#20585=CARTESIAN_POINT('Ctrl Pts',(0.166511139289342,1.06845992077163,1.28727233489076));
#20586=CARTESIAN_POINT('Ctrl Pts',(0.187915337510245,1.06442058969234,1.28796759655004));
#20587=CARTESIAN_POINT('Ctrl Pts',(0.209261745030533,1.06007279171241,1.2883190755065));
#20588=CARTESIAN_POINT('Ctrl Pts',(0.230552888394581,1.05542181279351,1.288319084765));
#20589=CARTESIAN_POINT('Ctrl Pts',(0.251712752465187,1.05079951139632,1.28831909396641));
#20590=CARTESIAN_POINT('Ctrl Pts',(0.272796801398367,1.04588243202759,1.28797193184368));
#20591=CARTESIAN_POINT('Ctrl Pts',(0.293809324770207,1.04067701160391,1.28727233489076));
#20592=CARTESIAN_POINT('Origin',(0.,0.,1.37171309575435));
#20593=CARTESIAN_POINT('',(0.500065917147839,1.15799828028598,1.10727038327973));
#20594=CARTESIAN_POINT('Ctrl Pts',(1.21572094522251,1.4127766116927,1.63615580822897));
#20595=CARTESIAN_POINT('Ctrl Pts',(1.13112438230172,1.42835456209775,1.59808263051822));
#20596=CARTESIAN_POINT('Ctrl Pts',(1.04649945489987,1.4332608863651,1.55687869031203));
#20597=CARTESIAN_POINT('Ctrl Pts',(0.863161299579016,1.41427936788009,1.4528510278119));
#20598=CARTESIAN_POINT('Ctrl Pts',(0.771992498477368,1.38392755544946,1.3904370872311));
#20599=CARTESIAN_POINT('Ctrl Pts',(0.614269670090823,1.2883224397548,1.25222975809873));
#20600=CARTESIAN_POINT('Ctrl Pts',(0.551263454538705,1.22690987286759,1.18062438818012));
#20601=CARTESIAN_POINT('Ctrl Pts',(0.500065917147839,1.15799828028598,1.10727038327973));
#20602=CARTESIAN_POINT('Origin',(0.,0.,1.10727038327973));
#20603=CARTESIAN_POINT('Ctrl Pts',(0.598371737951084,0.896396663228496,
1.28318517918604));
#20604=CARTESIAN_POINT('Ctrl Pts',(0.762485056494508,1.05584851328029,1.537509268581));
#20605=CARTESIAN_POINT('Ctrl Pts',(0.9783144252754,1.08712687701302,1.74606924121326));
#20606=CARTESIAN_POINT('Ctrl Pts',(1.24585984429376,0.99023175442669,1.90886509708284));
#20607=CARTESIAN_POINT('Ctrl Pts',(0.605275301161475,0.909465623084801,
1.26845681306972));
#20608=CARTESIAN_POINT('Ctrl Pts',(0.771441249464595,1.07130943365261,1.51984840181958));
#20609=CARTESIAN_POINT('Ctrl Pts',(0.990069682591161,1.10336947260001,1.72608377212012));
#20610=CARTESIAN_POINT('Ctrl Pts',(1.26141584343748,1.00546683912554,1.88700775532559));
#20611=CARTESIAN_POINT('Ctrl Pts',(0.621016981690702,0.932013737380381,
1.24112031232197));
#20612=CARTESIAN_POINT('Ctrl Pts',(0.791422088358104,1.09786234356421,1.48709491630374));
#20613=CARTESIAN_POINT('Ctrl Pts',(1.01568188386469,1.13056538342229,1.68880590632087));
#20614=CARTESIAN_POINT('Ctrl Pts',(1.29379626687143,1.03011319759961,1.846254814001));
#20615=CARTESIAN_POINT('Ctrl Pts',(0.673028944353636,0.971942506168049,
1.180578495595));
#20616=CARTESIAN_POINT('Ctrl Pts',(0.856136223676185,1.14383306000902,1.41443322333459));
#20617=CARTESIAN_POINT('Ctrl Pts',(1.09349602729721,1.17416051125987,1.60624275382306));
#20618=CARTESIAN_POINT('Ctrl Pts',(1.38525239147931,1.06283879403329,1.75591724097875));
#20619=CARTESIAN_POINT('Ctrl Pts',(0.726981684724074,0.994424673117319,
1.1340877844534));
#20620=CARTESIAN_POINT('Ctrl Pts',(0.922307368817381,1.16852049530615,1.35876508657128));
#20621=CARTESIAN_POINT('Ctrl Pts',(1.17034433001557,1.1937998639241,1.54303391436826));
#20622=CARTESIAN_POINT('Ctrl Pts',(1.47122482340644,1.0700086698298,1.68683916414419));
#20623=CARTESIAN_POINT('Ctrl Pts',(0.769660843866374,1.00715189764781,1.101666983688));
#20624=CARTESIAN_POINT('Ctrl Pts',(0.974320315501952,1.18199184824263,1.31997051162989));
#20625=CARTESIAN_POINT('Ctrl Pts',(1.23004502025839,1.20248619530708,1.4989879457606));
#20626=CARTESIAN_POINT('Ctrl Pts',(1.53683495813569,1.06863493884117,1.63871928608014));
#20627=CARTESIAN_POINT('',(0.601016155111926,0.89895057878464,1.28727233489076));
#20628=CARTESIAN_POINT('',(0.762339710524743,1.00491994924733,1.10727038327973));
#20629=CARTESIAN_POINT('Ctrl Pts',(0.601016155111926,0.89895057878464,1.28727233489076));
#20630=CARTESIAN_POINT('Ctrl Pts',(0.616327103756364,0.927868295879574,
1.25472274024271));
#20631=CARTESIAN_POINT('Ctrl Pts',(0.636369305963446,0.946670056291957,
1.2280379903142));
#20632=CARTESIAN_POINT('Ctrl Pts',(0.690422681622986,0.978914242873978,
1.1707920398759));
#20633=CARTESIAN_POINT('Ctrl Pts',(0.722616466757832,0.993317381306835,
1.14052203161603));
#20634=CARTESIAN_POINT('Ctrl Pts',(0.762339710524743,1.00491994924733,1.10727038327973));
#20635=CARTESIAN_POINT('Ctrl Pts',(0.601016155111926,0.89895057878464,1.28727233489076));
#20636=CARTESIAN_POINT('Ctrl Pts',(0.674061841710201,0.969072704191387,
1.39987124007464));
#20637=CARTESIAN_POINT('Ctrl Pts',(0.757283981982513,1.01397342270847,1.50346488650363));
#20638=CARTESIAN_POINT('Ctrl Pts',(0.966632999495317,1.05808377148838,1.715480776583));
#20639=CARTESIAN_POINT('Ctrl Pts',(1.09826755410688,1.04364312863621,1.81902921434248));
#20640=CARTESIAN_POINT('Ctrl Pts',(1.24558623976355,0.990330805779365,1.90869858745619));
#20641=CARTESIAN_POINT('Ctrl Pts',(0.762339710524743,1.00491994924733,1.10727038327973));
#20642=CARTESIAN_POINT('Ctrl Pts',(0.823177646383101,1.05844250017153,1.17697999301248));
#20643=CARTESIAN_POINT('Ctrl Pts',(0.894287935370968,1.10067719707671,1.24430717677952));
#20644=CARTESIAN_POINT('Ctrl Pts',(1.06468657657251,1.15446319222191,1.37795460947454));
#20645=CARTESIAN_POINT('Ctrl Pts',(1.15998911590306,1.16163314380192,1.43952296396723));
#20646=CARTESIAN_POINT('Ctrl Pts',(1.34351349395885,1.13824319621308,1.54471868724291));
#20647=CARTESIAN_POINT('Ctrl Pts',(1.43184312013697,1.11338277308098,1.59041399531275));
#20648=CARTESIAN_POINT('Ctrl Pts',(1.5239904260293,1.07301833748062,1.63615580822897));
#20649=CARTESIAN_POINT('Ctrl Pts',(0.498487526286222,1.16512557173636,1.10192461715937));
#20650=CARTESIAN_POINT('Ctrl Pts',(0.653828920782169,1.38489530661629,1.32030517702043));
#20651=CARTESIAN_POINT('Ctrl Pts',(0.896616198000952,1.46761240439959,1.49938098964775));
#20652=CARTESIAN_POINT('Ctrl Pts',(1.22684935794257,1.41327686508625,1.63915205504133));
#20653=CARTESIAN_POINT('Ctrl Pts',(0.508352002968308,1.12177948805866,1.13430265099724));
#20654=CARTESIAN_POINT('Ctrl Pts',(0.663777262634273,1.33220260121988,1.35904945381843));
#20655=CARTESIAN_POINT('Ctrl Pts',(0.901376560628895,1.40752683379662,1.54337045304295));
#20656=CARTESIAN_POINT('Ctrl Pts',(1.22117496033747,1.34801632954311,1.68721036521565));
#20657=CARTESIAN_POINT('Ctrl Pts',(0.515271529296697,1.06384346101581,1.18072933479299));
#20658=CARTESIAN_POINT('Ctrl Pts',(0.669611793063643,1.26193419272815,1.41464220917676));
#20659=CARTESIAN_POINT('Ctrl Pts',(0.899433473713048,1.32843484168648,1.60649429051817));
#20660=CARTESIAN_POINT('Ctrl Pts',(1.20484145605229,1.26345277789772,1.75619579796004));
#20661=CARTESIAN_POINT('Ctrl Pts',(0.506068760645491,0.999035931036402,
1.24118020602736));
#20662=CARTESIAN_POINT('Ctrl Pts',(0.655613152504221,1.18393656063858,1.48719644285888));
#20663=CARTESIAN_POINT('Ctrl Pts',(0.874439260092139,1.2429854225176,1.68893627188731));
#20664=CARTESIAN_POINT('Ctrl Pts',(1.1625431884408,1.17619191287087,1.84640112540367));
#20665=CARTESIAN_POINT('Ctrl Pts',(0.494188433189343,0.974277339819634,
1.26847955290007));
#20666=CARTESIAN_POINT('Ctrl Pts',(0.640153731237153,1.15458357076034,1.51990601315847));
#20667=CARTESIAN_POINT('Ctrl Pts',(0.853567659762739,1.21197995173255,1.72616419407531));
#20668=CARTESIAN_POINT('Ctrl Pts',(1.13460469485221,1.14668110494347,1.88709951781477));
#20669=CARTESIAN_POINT('Ctrl Pts',(0.486216000974361,0.961857913410637,
1.28318566992362));
#20670=CARTESIAN_POINT('Ctrl Pts',(0.629977719122416,1.13991207295831,1.5375404757467));
#20671=CARTESIAN_POINT('Ctrl Pts',(0.840512044007267,1.19691393144611,1.74612008846831));
#20672=CARTESIAN_POINT('Ctrl Pts',(1.11781897562892,1.13286348887405,1.90892450808844));
#20673=CARTESIAN_POINT('',(0.488533777383804,0.964710998256926,1.28727233489076));
#20674=CARTESIAN_POINT('Ctrl Pts',(0.500065917147839,1.15799828028598,1.10727038327973));
#20675=CARTESIAN_POINT('Ctrl Pts',(0.506409292188269,1.13262370376034,1.12805083925446));
#20676=CARTESIAN_POINT('Ctrl Pts',(0.511371411500265,1.10478303294993,1.1513125078925));
#20677=CARTESIAN_POINT('Ctrl Pts',(0.513808202166489,1.05860800687968,1.19194777349496));
#20678=CARTESIAN_POINT('Ctrl Pts',(0.513729024230259,1.03731460867027,1.2110848927995));
#20679=CARTESIAN_POINT('Ctrl Pts',(0.507067244033061,1.00241946522318,1.24526606650694));
#20680=CARTESIAN_POINT('Ctrl Pts',(0.501447516417269,0.984791876090262,
1.26352342884106));
#20681=CARTESIAN_POINT('Ctrl Pts',(0.488533777383804,0.964710998256926,
1.28727233489076));
#20682=CARTESIAN_POINT('Ctrl Pts',(0.488533777383804,0.964710998256926,
1.28727233489076));
#20683=CARTESIAN_POINT('Ctrl Pts',(0.552615413818275,1.04310952295002,1.39987124007464));
#20684=CARTESIAN_POINT('Ctrl Pts',(0.629833086622262,1.09769367964031,1.50346488650363));
#20685=CARTESIAN_POINT('Ctrl Pts',(0.832357123065218,1.16666286599128,1.715480776583));
#20686=CARTESIAN_POINT('Ctrl Pts',(0.964772942765737,1.16815913695893,1.81902921434248));
#20687=CARTESIAN_POINT('Ctrl Pts',(1.11743425489732,1.13295228123076,1.90869858745619));
#20688=CARTESIAN_POINT('Ctrl Pts',(0.488533777383804,0.964710998256926,
1.28727233489076));
#20689=CARTESIAN_POINT('Ctrl Pts',(0.632616760336964,1.14098448197888,1.54044293163017));
#20690=CARTESIAN_POINT('Ctrl Pts',(0.843108069941918,1.19686606932897,1.74808806329354));
#20691=CARTESIAN_POINT('Ctrl Pts',(1.12000770619867,1.13235576030722,1.91020772988088));
#20692=CARTESIAN_POINT('Ctrl Pts',(0.526027903293178,0.94279085843283,1.28727233489076));
#20693=CARTESIAN_POINT('Ctrl Pts',(0.676829228446517,1.11286137791709,1.54044293163017));
#20694=CARTESIAN_POINT('Ctrl Pts',(0.889051558128351,1.16016893831867,1.74808806329354));
#20695=CARTESIAN_POINT('Ctrl Pts',(1.16269489233868,1.08471353963759,1.91020772988088));
#20696=CARTESIAN_POINT('Ctrl Pts',(0.563522029202552,0.920870718608735,
1.28727233489076));
#20697=CARTESIAN_POINT('Ctrl Pts',(0.72104169655607,1.0847382738553,1.54044293163017));
#20698=CARTESIAN_POINT('Ctrl Pts',(0.934995046314783,1.12347180730837,1.74808806329354));
#20699=CARTESIAN_POINT('Ctrl Pts',(1.20538207847869,1.03707131896797,1.91020772988088));
#20700=CARTESIAN_POINT('Ctrl Pts',(0.601016155111926,0.89895057878464,1.28727233489076));
#20701=CARTESIAN_POINT('Ctrl Pts',(0.765254164665624,1.05661516979351,1.54044293163017));
#20702=CARTESIAN_POINT('Ctrl Pts',(0.980938534501216,1.08677467629807,1.74808806329354));
#20703=CARTESIAN_POINT('Ctrl Pts',(1.2480692646187,0.989429098298345,1.91020772988088));
#20704=CARTESIAN_POINT('Ctrl Pts',(0.488533777383804,0.964710998256926,
1.28727233489076));
#20705=CARTESIAN_POINT('Ctrl Pts',(0.507642157628461,0.95425510511126,1.28796759655004));
#20706=CARTESIAN_POINT('Ctrl Pts',(0.526600254136213,0.943523700818289,
1.2883190755065));
#20707=CARTESIAN_POINT('Ctrl Pts',(0.545412103245543,0.932521031881151,
1.288319084765));
#20708=CARTESIAN_POINT('Ctrl Pts',(0.564107960168948,0.921586204420606,
1.28831909396641));
#20709=CARTESIAN_POINT('Ctrl Pts',(0.582640621209095,0.910394454615255,
1.28797193184368));
#20710=CARTESIAN_POINT('Ctrl Pts',(0.601016155111926,0.89895057878464,1.28727233489076));
#20711=CARTESIAN_POINT('Origin',(0.,0.,1.37171309575435));
#20712=CARTESIAN_POINT('',(0.833432097145896,0.946792943618189,1.10727038327973));
#20713=CARTESIAN_POINT('Ctrl Pts',(1.59279130921887,0.967951970128403,1.63615580822897));
#20714=CARTESIAN_POINT('Ctrl Pts',(1.51714904820957,1.00890925697988,1.59808263051822));
#20715=CARTESIAN_POINT('Ctrl Pts',(1.43818209714157,1.03972598936032,1.55687869031203));
#20716=CARTESIAN_POINT('Ctrl Pts',(1.25795153804723,1.07832809822746,1.45285102781191));
#20717=CARTESIAN_POINT('Ctrl Pts',(1.16186562982555,1.07763451813115,1.39043708723111));
#20718=CARTESIAN_POINT('Ctrl Pts',(0.982318700621182,1.03544768423092,1.25222975809873));
#20719=CARTESIAN_POINT('Ctrl Pts',(0.903418701916906,0.996510853667278,
1.18062438818012));
#20720=CARTESIAN_POINT('Ctrl Pts',(0.833432097145897,0.946792943618189,
1.10727038327973));
#20721=CARTESIAN_POINT('Origin',(0.,0.,1.10727038327973));
#20722=CARTESIAN_POINT('Ctrl Pts',(0.846087143183836,0.667616851768136,
1.28318517918604));
#20723=CARTESIAN_POINT('Ctrl Pts',(1.05144151564591,0.768550768362022,1.53750926858099));
#20724=CARTESIAN_POINT('Ctrl Pts',(1.2663729891825,0.731603317170575,1.74606924121326));
#20725=CARTESIAN_POINT('Ctrl Pts',(1.4908815637936,0.556774498193796,1.90886509708283));
#20726=CARTESIAN_POINT('Ctrl Pts',(0.856691352655137,0.677912852846922,
1.26845681306972));
#20727=CARTESIAN_POINT('Ctrl Pts',(1.06473704847503,0.780487361597376,1.51984840181957));
#20728=CARTESIAN_POINT('Ctrl Pts',(1.28257214132252,0.743418369261302,1.72608377212011));
#20729=CARTESIAN_POINT('Ctrl Pts',(1.51038409822941,0.56645685667305,1.88700775532558));
#20730=CARTESIAN_POINT('Ctrl Pts',(0.878631748253099,0.694492950134685,
1.24111924840996));
#20731=CARTESIAN_POINT('Ctrl Pts',(1.0919466731633,0.799566273875776,1.48709385239173));
#20732=CARTESIAN_POINT('Ctrl Pts',(1.31533666464122,0.761367941758637,1.68880445881716));
#20733=CARTESIAN_POINT('Ctrl Pts',(1.54879772833386,0.579890165126711,1.84625336649728));
#20734=CARTESIAN_POINT('Ctrl Pts',(0.940438249469778,0.716394511678359,
1.18057655035131));
#20735=CARTESIAN_POINT('Ctrl Pts',(1.16770072295995,0.823288881893969,1.4144312780909));
#20736=CARTESIAN_POINT('Ctrl Pts',(1.40281580396031,0.778782224872496,1.60624011348192));
#20737=CARTESIAN_POINT('Ctrl Pts',(1.64589229282025,0.582751305549679,1.75591460063761));
#20738=CARTESIAN_POINT('Ctrl Pts',(0.998694792103065,0.72110437015383,1.1340877844534));
#20739=CARTESIAN_POINT('Ctrl Pts',(1.23825912446584,0.82632038048354,1.35876508657128));
#20740=CARTESIAN_POINT('Ctrl Pts',(1.48196804720543,0.773714852492098,1.54303391436825));
#20741=CARTESIAN_POINT('Ctrl Pts',(1.7298688183418,0.563005244955071,1.68683916414418));
#20742=CARTESIAN_POINT('Ctrl Pts',(1.0432180131865,0.720020094497306,1.101666983688));
#20743=CARTESIAN_POINT('Ctrl Pts',(1.29188925333651,0.823059514024041,1.31997051162989));
#20744=CARTESIAN_POINT('Ctrl Pts',(1.54143100170431,0.76352751669565,1.4989879457606));
#20745=CARTESIAN_POINT('Ctrl Pts',(1.79184325828988,0.541424102512133,1.63871928608013));
#20746=CARTESIAN_POINT('',(0.849391336665505,0.669228599956957,1.28727233489076));
#20747=CARTESIAN_POINT('',(1.03556549162895,0.720159740047643,1.10727038327973));
#20748=CARTESIAN_POINT('Ctrl Pts',(0.849391336665505,0.669228599956957,
1.28727233489076));
#20749=CARTESIAN_POINT('Ctrl Pts',(0.872888980165507,0.691999639905522,
1.25472274024245));
#20750=CARTESIAN_POINT('Ctrl Pts',(0.897760310667753,0.703687795576912,
1.22803799031335));
#20751=CARTESIAN_POINT('Ctrl Pts',(0.959132127441248,0.717650427656427,
1.17079203987406));
#20752=CARTESIAN_POINT('Ctrl Pts',(0.994201051126515,0.721400199597683,
1.14052203161404));
#20753=CARTESIAN_POINT('Ctrl Pts',(1.03556549162895,0.720159740047643,1.10727038327973));
#20754=CARTESIAN_POINT('Ctrl Pts',(0.849391336665505,0.669228599956957,
1.28727233489076));
#20755=CARTESIAN_POINT('Ctrl Pts',(0.940530841324424,0.713346345736856,
1.39987124007464));
#20756=CARTESIAN_POINT('Ctrl Pts',(1.03355488521186,0.73033241101646,1.50346488650363));
#20757=CARTESIAN_POINT('Ctrl Pts',(1.2462884798982,0.707591441492496,1.715480776583));
#20758=CARTESIAN_POINT('Ctrl Pts',(1.36701797678012,0.653180259586497,1.81902921434248));
#20759=CARTESIAN_POINT('Ctrl Pts',(1.49065195897357,0.556953250077769,1.90869858745619));
#20760=CARTESIAN_POINT('Ctrl Pts',(1.03556549162895,0.720159740047643,1.10727038327973));
#20761=CARTESIAN_POINT('Ctrl Pts',(1.10996518478287,0.752262754789917,1.17697999301248));
#20762=CARTESIAN_POINT('Ctrl Pts',(1.19064632759639,0.77045605072318,1.24430717677953));
#20763=CARTESIAN_POINT('Ctrl Pts',(1.3693258522382,0.768953495941755,1.37795460947454));
#20764=CARTESIAN_POINT('Ctrl Pts',(1.46217959017505,0.746322420853228,1.43952296396723));
#20765=CARTESIAN_POINT('Ctrl Pts',(1.62949375452144,0.667365107081762,1.54471868724285));
#20766=CARTESIAN_POINT('Ctrl Pts',(1.70581792784489,0.616426084068337,1.5904139953127));
#20767=CARTESIAN_POINT('Ctrl Pts',(1.78098192700405,0.549562141057365,1.63615580822897));
#20768=CARTESIAN_POINT('Ctrl Pts',(0.834133412413726,0.954059150195613,
1.10192461715937));
#20769=CARTESIAN_POINT('Ctrl Pts',(1.04978444082665,1.11506945780848,1.32030517702044));
#20770=CARTESIAN_POINT('Ctrl Pts',(1.30624985183956,1.11871269798568,1.49938098964776));
#20771=CARTESIAN_POINT('Ctrl Pts',(1.60352964545243,0.964988870727209,1.63915205504134));
#20772=CARTESIAN_POINT('Ctrl Pts',(0.831123661162973,0.920854500490908,
1.12620814253777));
#20773=CARTESIAN_POINT('Ctrl Pts',(1.04468843542397,1.0751219753964,1.34937307009661));
#20774=CARTESIAN_POINT('Ctrl Pts',(1.29577263793342,1.07480228609568,1.5323675387164));
#20775=CARTESIAN_POINT('Ctrl Pts',(1.58435717993001,0.919754141507906,1.67519578767208));
#20776=CARTESIAN_POINT('Ctrl Pts',(0.821762669862007,0.868512346714967,
1.16792406090532));
#20777=CARTESIAN_POINT('Ctrl Pts',(1.0310896536259,1.01237142622958,1.39930793834175));
#20778=CARTESIAN_POINT('Ctrl Pts',(1.27300639515449,1.00637513236489,1.589090429871));
#20779=CARTESIAN_POINT('Ctrl Pts',(1.54763812191341,0.850420920292676,1.7371752932628));
#20780=CARTESIAN_POINT('Ctrl Pts',(0.79788991722713,0.804559127620147,1.22814985715448));
#20781=CARTESIAN_POINT('Ctrl Pts',(0.999388130632025,0.93612497529341,1.4715455490462));
#20782=CARTESIAN_POINT('Ctrl Pts',(1.22846526028813,0.924963031592628,1.67113688711451));
#20783=CARTESIAN_POINT('Ctrl Pts',(1.48512921647049,0.771080298579199,1.82691809308167));
#20784=CARTESIAN_POINT('Ctrl Pts',(0.774876067377614,0.776996174893135,
1.26357751389222));
#20785=CARTESIAN_POINT('Ctrl Pts',(0.97038356235556,0.903792375271581,1.51402822523203));
#20786=CARTESIAN_POINT('Ctrl Pts',(1.19205686236993,0.892403735624943,1.71951214242026));
#20787=CARTESIAN_POINT('Ctrl Pts',(1.44016181895954,0.742597824795289,1.87982452105689));
#20788=CARTESIAN_POINT('Ctrl Pts',(0.75964933747155,0.764532229061143,1.28318566992362));
#20789=CARTESIAN_POINT('Ctrl Pts',(0.951396617529429,0.889446983704126,
1.53754047574671));
#20790=CARTESIAN_POINT('Ctrl Pts',(1.16924120209866,0.878600288371208,1.74612008846832));
#20791=CARTESIAN_POINT('Ctrl Pts',(1.41318309117925,0.731992143062389,1.90892450808845));
#20792=CARTESIAN_POINT('',(0.762735325532963,0.766529441696069,1.28727233489076));
#20793=CARTESIAN_POINT('Ctrl Pts',(0.833432097145897,0.946792943618189,
1.10727038327973));
#20794=CARTESIAN_POINT('Ctrl Pts',(0.831623829941911,0.920700076576089,
1.12805083925443));
#20795=CARTESIAN_POINT('Ctrl Pts',(0.827739845433,0.892688645988255,1.15131250789251));
#20796=CARTESIAN_POINT('Ctrl Pts',(0.815788503303407,0.848020576825928,
1.19194777349545));
#20797=CARTESIAN_POINT('Ctrl Pts',(0.809133178696474,0.827793819032885,
1.21108489279985));
#20798=CARTESIAN_POINT('Ctrl Pts',(0.792014256883229,0.796665168763711,
1.24526606650783));
#20799=CARTESIAN_POINT('Ctrl Pts',(0.781222353702368,0.78163692658966,1.2635234288418));
#20800=CARTESIAN_POINT('Ctrl Pts',(0.762735325532963,0.766529441696069,
1.28727233489076));
#20801=CARTESIAN_POINT('Ctrl Pts',(0.762735325532963,0.766529441696069,
1.28727233489076));
#20802=CARTESIAN_POINT('Ctrl Pts',(0.847907059902912,0.821288554787752,
1.39987124007464));
#20803=CARTESIAN_POINT('Ctrl Pts',(0.938212862837218,0.849339599532016,
1.50346488650363));
#20804=CARTESIAN_POINT('Ctrl Pts',(1.15213731807335,0.852349824604395,1.715480776583));
#20805=CARTESIAN_POINT('Ctrl Pts',(1.27853461941729,0.812854124246773,1.81902921434248));
#20806=CARTESIAN_POINT('Ctrl Pts',(1.41284463836769,0.732195474855992,1.90869858745619));
#20807=CARTESIAN_POINT('Ctrl Pts',(0.762735325532963,0.766529441696069,
1.28727233489076));
#20808=CARTESIAN_POINT('Ctrl Pts',(0.954237887485568,0.889651396707116,
1.54044293163017));
#20809=CARTESIAN_POINT('Ctrl Pts',(1.17169537927269,0.877752552661174,1.74808806329354));
#20810=CARTESIAN_POINT('Ctrl Pts',(1.41510780089433,0.730832909558243,1.91020772988088));
#20811=CARTESIAN_POINT('Ctrl Pts',(0.791620662577143,0.734095827783032,
1.28727233489076));
#20812=CARTESIAN_POINT('Ctrl Pts',(0.987595926292982,0.849242331321592,
1.54044293163017));
#20813=CARTESIAN_POINT('Ctrl Pts',(1.20405019596674,0.828654188454019,1.74808806329354));
#20814=CARTESIAN_POINT('Ctrl Pts',(1.44098347159841,0.672331399180314,1.91020772988088));
#20815=CARTESIAN_POINT('Ctrl Pts',(0.820505999621324,0.701662213869994,
1.28727233489076));
#20816=CARTESIAN_POINT('Ctrl Pts',(1.0209539651004,0.808833265936067,1.54044293163017));
#20817=CARTESIAN_POINT('Ctrl Pts',(1.23640501266079,0.779555824246864,1.74808806329354));
#20818=CARTESIAN_POINT('Ctrl Pts',(1.4668591423025,0.613829888802385,1.91020772988088));
#20819=CARTESIAN_POINT('Ctrl Pts',(0.849391336665505,0.669228599956957,
1.28727233489076));
#20820=CARTESIAN_POINT('Ctrl Pts',(1.05431200390781,0.768424200550542,1.54044293163017));
#20821=CARTESIAN_POINT('Ctrl Pts',(1.26875982935484,0.730457460039708,1.74808806329354));
#20822=CARTESIAN_POINT('Ctrl Pts',(1.49273481300659,0.555328378424457,1.91020772988088));
#20823=CARTESIAN_POINT('Ctrl Pts',(0.762735325532963,0.766529441696069,
1.28727233489076));
#20824=CARTESIAN_POINT('Ctrl Pts',(0.777677426407088,0.750680482155644,
1.28796759655004));
#20825=CARTESIAN_POINT('Ctrl Pts',(0.792391461327313,0.734615936171909,
1.2883190755065));
#20826=CARTESIAN_POINT('Ctrl Pts',(0.806882581321256,0.718338595112193,
1.288319084765));
#20827=CARTESIAN_POINT('Ctrl Pts',(0.82128435036013,0.702161618687529,1.28831909396641));
#20828=CARTESIAN_POINT('Ctrl Pts',(0.835451517520018,0.685790724893994,
1.28797193184368));
#20829=CARTESIAN_POINT('Ctrl Pts',(0.849391336665505,0.669228599956957,
1.28727233489076));
#20830=CARTESIAN_POINT('Origin',(0.,0.,1.37171309575435));
#20831=CARTESIAN_POINT('',(1.08521613661244,0.642908916934715,1.10727038327973));
#20832=CARTESIAN_POINT('Ctrl Pts',(1.81394816223928,0.428377445609997,1.63615580822897));
#20833=CARTESIAN_POINT('Ctrl Pts',(1.75466459467969,0.490704884304684,1.59808263051822));
#20834=CARTESIAN_POINT('Ctrl Pts',(1.68908545531116,0.544415468320014,1.55687869031203));
#20835=CARTESIAN_POINT('Ctrl Pts',(1.52960471530762,0.636822561166699,1.4528510278119));
#20836=CARTESIAN_POINT('Ctrl Pts',(1.43800725813253,0.665855105856973,1.39043708723109));
#20837=CARTESIAN_POINT('Ctrl Pts',(1.25421153251789,0.681216094986277,1.25222975809873));
#20838=CARTESIAN_POINT('Ctrl Pts',(1.16714103226326,0.668566409010631,1.18062438818012));
#20839=CARTESIAN_POINT('Ctrl Pts',(1.08521613661244,0.642908916934714,1.10727038327973));
#20840=CARTESIAN_POINT('Origin',(0.,0.,1.10727038327973));
#20841=CARTESIAN_POINT('Ctrl Pts',(1.08812850838495,0.649602771712747,1.10192461715937));
#20842=CARTESIAN_POINT('Ctrl Pts',(1.34297974552472,0.736092841324622,1.32030517702043));
#20843=CARTESIAN_POINT('Ctrl Pts',(1.58801866900219,0.660305598163242,1.49938098964775));
#20844=CARTESIAN_POINT('Ctrl Pts',(1.82324527881736,0.422241042228606,1.63915205504132));
#20845=CARTESIAN_POINT('Ctrl Pts',(1.07063084893098,0.608736859462564,1.13430265099723));
#20846=CARTESIAN_POINT('Ctrl Pts',(1.32005612801352,0.687616058553887,1.35904945381841));
#20847=CARTESIAN_POINT('Ctrl Pts',(1.55655247099158,0.608897279480441,1.54337045304294));
#20848=CARTESIAN_POINT('Ctrl Pts',(1.78029541437302,0.37277948714011,1.68721036521563));
#20849=CARTESIAN_POINT('Ctrl Pts',(1.04217626136028,0.557802714124105,1.18072639205178));
#20850=CARTESIAN_POINT('Ctrl Pts',(1.28347496838039,0.62734255163042,1.41463926643554));
#20851=CARTESIAN_POINT('Ctrl Pts',(1.50849481334977,0.546058002751389,1.6064902962218));
#20852=CARTESIAN_POINT('Ctrl Pts',(1.71737956252142,0.313972100865329,1.75619180366366));
#20853=CARTESIAN_POINT('Ctrl Pts',(0.996637718803135,0.510779237881579,
1.24117859886916));
#20854=CARTESIAN_POINT('Ctrl Pts',(1.22630353645006,0.572467001402756,1.48719483570068));
#20855=CARTESIAN_POINT('Ctrl Pts',(1.43804667102142,0.491616133252199,1.68893408523068));
#20856=CARTESIAN_POINT('Ctrl Pts',(1.63186740528246,0.268235808623187,1.84639893874703));
#20857=CARTESIAN_POINT('Ctrl Pts',(0.972472692862429,0.497730252266281,
1.26847955290007));
#20858=CARTESIAN_POINT('Ctrl Pts',(1.1965424430155,0.557804807750029,1.51990601315847));
#20859=CARTESIAN_POINT('Ctrl Pts',(1.40293468429944,0.478797895551027,1.7261641940753));
#20860=CARTESIAN_POINT('Ctrl Pts',(1.59191672260124,0.260780594211983,1.88709951781476));
#20861=CARTESIAN_POINT('Ctrl Pts',(0.958722904028867,0.49236880332188,1.28318566992362));
#20862=CARTESIAN_POINT('Ctrl Pts',(1.17968618624263,0.55191662654344,1.5375404757467));
#20863=CARTESIAN_POINT('Ctrl Pts',(1.38351688474613,0.474283127502366,1.7461200884683));
#20864=CARTESIAN_POINT('Ctrl Pts',(1.57021499953935,0.259468306198656,1.90892450808844));
#20865=CARTESIAN_POINT('',(0.962275025729455,0.493314642657339,1.28727233489076));
#20866=CARTESIAN_POINT('Ctrl Pts',(0.962275025729455,0.493314642657339,
1.28727233489076));
#20867=CARTESIAN_POINT('Ctrl Pts',(1.06019965524839,0.519074140629024,1.39987124007464));
#20868=CARTESIAN_POINT('Ctrl Pts',(1.15475382712427,0.517846241724568,1.50346488650363));
#20869=CARTESIAN_POINT('Ctrl Pts',(1.35913828497575,0.454602843714802,1.715480776583));
#20870=CARTESIAN_POINT('Ctrl Pts',(1.46714441944577,0.377981286365636,1.81902921434248));
#20871=CARTESIAN_POINT('Ctrl Pts',(1.5699559447672,0.259766273896473,1.90869858745619));
#20872=CARTESIAN_POINT('Ctrl Pts',(1.08521613661244,0.642908916934714,1.10727038327973));
#20873=CARTESIAN_POINT('Ctrl Pts',(1.0754332329569,0.618651911001869,1.12805083925446));
#20874=CARTESIAN_POINT('Ctrl Pts',(1.06308333609211,0.593211674629706,1.15131250789255));
#20875=CARTESIAN_POINT('Ctrl Pts',(1.03791374180399,0.554422984205844,1.19194777349584));
#20876=CARTESIAN_POINT('Ctrl Pts',(1.02533374006937,0.537242802810037,1.21108489280014));
#20877=CARTESIAN_POINT('Ctrl Pts',(0.999433395982306,0.512927734894202,
1.24526606650747));
#20878=CARTESIAN_POINT('Ctrl Pts',(0.984525703911604,0.501969908730509,
1.26352342884146));
#20879=CARTESIAN_POINT('Ctrl Pts',(0.962275025729455,0.493314642657339,
1.28727233489076));
#20880=CARTESIAN_POINT('Ctrl Pts',(0.962275025729455,0.493314642657339,
1.28727233489076));
#20881=CARTESIAN_POINT('Ctrl Pts',(1.18245156164078,0.551233034159898,1.54044293163017));
#20882=CARTESIAN_POINT('Ctrl Pts',(1.38558898119851,0.472718500477254,1.74808806329354));
#20883=CARTESIAN_POINT('Ctrl Pts',(1.57168728440264,0.257771041609407,1.91020772988088));
#20884=CARTESIAN_POINT('Ctrl Pts',(0.979724075862581,0.453542382763444,
1.28727233489076));
#20885=CARTESIAN_POINT('Ctrl Pts',(1.20168985388846,0.502493528317088,1.54044293163017));
#20886=CARTESIAN_POINT('Ctrl Pts',(1.40118801151289,0.416024993050259,1.74808806329354));
#20887=CARTESIAN_POINT('Ctrl Pts',(1.57821854873589,0.194136776962957,1.91020772988088));
#20888=CARTESIAN_POINT('Ctrl Pts',(0.997173125995706,0.413770122869549,
1.28727233489076));
#20889=CARTESIAN_POINT('Ctrl Pts',(1.22092814613614,0.453754022474278,1.54044293163017));
#20890=CARTESIAN_POINT('Ctrl Pts',(1.41678704182728,0.359331485623264,1.74808806329354));
#20891=CARTESIAN_POINT('Ctrl Pts',(1.58474981306913,0.130502512316507,1.91020772988088));
#20892=CARTESIAN_POINT('Ctrl Pts',(1.01462217612883,0.373997862975653,1.28727233489076));
#20893=CARTESIAN_POINT('Ctrl Pts',(1.24016643838382,0.405014516631468,1.54044293163017));
#20894=CARTESIAN_POINT('Ctrl Pts',(1.43238607214167,0.302637978196269,1.74808806329354));
#20895=CARTESIAN_POINT('Ctrl Pts',(1.59128107740238,0.0668682476700567,
1.91020772988088));
#20896=CARTESIAN_POINT('',(1.01462217612883,0.373997862975654,1.28727233489076));
#20897=CARTESIAN_POINT('Ctrl Pts',(1.01462217612883,0.373997862975653,1.28727233489076));
#20898=CARTESIAN_POINT('Ctrl Pts',(1.11493412912611,0.387792676785359,1.39987124007464));
#20899=CARTESIAN_POINT('Ctrl Pts',(1.20865423507634,0.375201374409042,1.50346488650363));
#20900=CARTESIAN_POINT('Ctrl Pts',(1.40394856048621,0.287835131123856,1.715480776583));
#20901=CARTESIAN_POINT('Ctrl Pts',(1.50195515531182,0.198779555753984,1.81902921434248));
#20902=CARTESIAN_POINT('Ctrl Pts',(1.58980227845634,0.0690572297370882,
1.90869858745619));
#20903=CARTESIAN_POINT('Ctrl Pts',(0.962275025729455,0.493314642657339,
1.28727233489076));
#20904=CARTESIAN_POINT('Ctrl Pts',(0.971588210291788,0.473624023308133,
1.28796759655004));
#20905=CARTESIAN_POINT('Ctrl Pts',(0.980617871367766,0.453798845322811,
1.2883190755065));
#20906=CARTESIAN_POINT('Ctrl Pts',(0.989369770455727,0.433840171694363,
1.288319084765));
#20907=CARTESIAN_POINT('Ctrl Pts',(0.9980677061135,0.414004561469663,1.28831909396641));
#20908=CARTESIAN_POINT('Ctrl Pts',(1.00648259836304,0.394057020835195,1.28797193184368));
#20909=CARTESIAN_POINT('Ctrl Pts',(1.01462217612883,0.373997862975653,1.28727233489076));
#20910=CARTESIAN_POINT('Ctrl Pts',(1.01098164380599,0.373486051296587,1.28318517918604));
#20911=CARTESIAN_POINT('Ctrl Pts',(1.23747555342208,0.40602191942841,1.53750926858099));
#20912=CARTESIAN_POINT('Ctrl Pts',(1.43047014156898,0.304465327263434,1.74606924121325));
#20913=CARTESIAN_POINT('Ctrl Pts',(1.58996540824668,0.0688162748016592,
1.90886509708283));
#20914=CARTESIAN_POINT('Ctrl Pts',(1.02865698469238,0.382166213971436,1.26356265747109));
#20915=CARTESIAN_POINT('Ctrl Pts',(1.25921979945503,0.415747810278511,1.51398032870897));
#20916=CARTESIAN_POINT('Ctrl Pts',(1.45578649927554,0.312707553760741,1.71944252353203));
#20917=CARTESIAN_POINT('Ctrl Pts',(1.61866306691266,0.0730554435692883,
1.87974468006743));
#20918=CARTESIAN_POINT('Ctrl Pts',(1.06331677531061,0.391657241669877,1.2281080635226));
#20919=CARTESIAN_POINT('Ctrl Pts',(1.30153367691801,0.425647906592844,1.47146671103428));
#20920=CARTESIAN_POINT('Ctrl Pts',(1.50438827167772,0.318676377131993,1.67103178775815));
#20921=CARTESIAN_POINT('Ctrl Pts',(1.67188067012362,0.0707311879561156,
1.82679988540377));
#20922=CARTESIAN_POINT('Ctrl Pts',(1.13146507111568,0.386793101125271,1.16783895333641));
#20923=CARTESIAN_POINT('Ctrl Pts',(1.38370624635607,0.41672899565074,1.39917869757247));
#20924=CARTESIAN_POINT('Ctrl Pts',(1.59505828371836,0.298796521842133,1.5889289477722));
#20925=CARTESIAN_POINT('Ctrl Pts',(1.76565888855501,0.032993380760367,1.73699566095832));
#20926=CARTESIAN_POINT('Ctrl Pts',(1.18300585575676,0.373540819382844,1.12609865864079));
#20927=CARTESIAN_POINT('Ctrl Pts',(1.44530457310529,0.398429005793492,1.34921513358856));
#20928=CARTESIAN_POINT('Ctrl Pts',(1.66164003747217,0.270901963247261,1.53217466057835));
#20929=CARTESIAN_POINT('Ctrl Pts',(1.83206393610153,-0.00890514499182499,
1.67498164591399));
#20930=CARTESIAN_POINT('Ctrl Pts',(1.21448591285885,0.362468171451202,1.10179959977345));
#20931=CARTESIAN_POINT('Ctrl Pts',(1.48279448162748,0.383640993960512,1.32012924726704));
#20932=CARTESIAN_POINT('Ctrl Pts',(1.70171239168859,0.249943984819042,1.49916808705051));
#20933=CARTESIAN_POINT('Ctrl Pts',(1.87123964304218,-0.0386228559732111,
1.63891611912387));
#20934=CARTESIAN_POINT('',(1.20742290720348,0.364905277844141,1.10727038327973));
#20935=CARTESIAN_POINT('Ctrl Pts',(1.20742290720348,0.364905277844141,1.10727038327973));
#20936=CARTESIAN_POINT('Ctrl Pts',(1.2881015973139,0.372446289646659,1.17697999301248));
#20937=CARTESIAN_POINT('Ctrl Pts',(1.3704559615559,0.364817298041905,1.24430717677952));
#20938=CARTESIAN_POINT('Ctrl Pts',(1.53992597283256,0.308173273864794,1.37795460947453));
#20939=CARTESIAN_POINT('Ctrl Pts',(1.62124173855644,0.257956459417363,1.43952296396722));
#20940=CARTESIAN_POINT('Ctrl Pts',(1.75990988600071,0.127450637982172,1.547796704752));
#20941=CARTESIAN_POINT('Ctrl Pts',(1.81609416413933,0.0535283678677367,
1.5933649555937));
#20942=CARTESIAN_POINT('Ctrl Pts',(1.86363850813291,-0.0276890267571701,
1.63615580822897));
#20943=CARTESIAN_POINT('Ctrl Pts',(1.01462217612883,0.373997862975653,1.28727233489076));
#20944=CARTESIAN_POINT('Ctrl Pts',(1.0440064014209,0.388393237732341,1.25472274024233));
#20945=CARTESIAN_POINT('Ctrl Pts',(1.07127228109912,0.391823670549181,1.22803799031345));
#20946=CARTESIAN_POINT('Ctrl Pts',(1.13395503796013,0.386137988414013,1.1707920398715));
#20947=CARTESIAN_POINT('Ctrl Pts',(1.16846630960532,0.378867340059468,1.14052203161166));
#20948=CARTESIAN_POINT('Ctrl Pts',(1.20742290720348,0.364905277844141,1.10727038327973));
#20949=CARTESIAN_POINT('Ctrl Pts',(1.23578335387376,0.281756991007075,1.1017328493151));
#20950=CARTESIAN_POINT('Ctrl Pts',(1.50493278576872,0.285293785520307,1.3200756344191));
#20951=CARTESIAN_POINT('Ctrl Pts',(1.71461214828353,0.137495264840185,1.49912049044759));
#20952=CARTESIAN_POINT('Ctrl Pts',(1.86482144141819,-0.16163857103329,1.63886741740055));
#20953=CARTESIAN_POINT('Ctrl Pts',(1.20648752589176,0.248240087990173,1.13414277848452));
#20954=CARTESIAN_POINT('Ctrl Pts',(1.46811671142948,0.246204407588735,1.35885799576156));
#20955=CARTESIAN_POINT('Ctrl Pts',(1.66875380764494,0.0982540365453173,
1.54315303441877));
#20956=CARTESIAN_POINT('Ctrl Pts',(1.80862652874333,-0.195476545731338,
1.68697274180732));
#20957=CARTESIAN_POINT('Ctrl Pts',(1.16364558145094,0.2085271896007,1.1806131496188));
#20958=CARTESIAN_POINT('Ctrl Pts',(1.41464853624076,0.20010880260165,1.41450373020722));
#20959=CARTESIAN_POINT('Ctrl Pts',(1.60356331755514,0.053262188267234,1.60633610108347));
#20960=CARTESIAN_POINT('Ctrl Pts',(1.73053166984717,-0.232035965773771,
1.75602333097544));
#20961=CARTESIAN_POINT('Ctrl Pts',(1.10574232216633,0.177813888094452,1.24113368360636));
#20962=CARTESIAN_POINT('Ctrl Pts',(1.34323970181785,0.165512243823414,1.48714102989093));
#20963=CARTESIAN_POINT('Ctrl Pts',(1.51964328480289,0.0231812731496048,
1.68887271819552));
#20964=CARTESIAN_POINT('Ctrl Pts',(1.63495516880573,-0.249170413362414,
1.84633185797667));
#20965=CARTESIAN_POINT('Ctrl Pts',(1.07870022090367,0.172859970247478,1.26846296103996));
#20966=CARTESIAN_POINT('Ctrl Pts',(1.31037084404559,0.160752258036383,1.51988605935311));
#20967=CARTESIAN_POINT('Ctrl Pts',(1.48224938444032,0.0218314126094617,
1.72614171343828));
#20968=CARTESIAN_POINT('Ctrl Pts',(1.59461215150753,-0.243918395495164,
1.88707489423908));
#20969=CARTESIAN_POINT('Ctrl Pts',(1.06394999292458,0.172008888578299,1.28318566992362));
#20970=CARTESIAN_POINT('Ctrl Pts',(1.29249985168945,0.160360824547434,1.5375404757467));
#20971=CARTESIAN_POINT('Ctrl Pts',(1.46236429518571,0.0235398295887289,
1.74612008846831));
#20972=CARTESIAN_POINT('Ctrl Pts',(1.57354332341336,-0.238454096297817,
1.90892450808844));
#20973=CARTESIAN_POINT('',(1.06762054184321,0.171810769270086,1.28727233489076));
#20974=CARTESIAN_POINT('Ctrl Pts',(1.06762054184321,0.171810769270086,1.28727233489076));
#20975=CARTESIAN_POINT('Ctrl Pts',(1.16871252149279,0.166049132983329,1.39987124007464));
#20976=CARTESIAN_POINT('Ctrl Pts',(1.25825944116939,0.135662485730195,1.50346488650363));
#20977=CARTESIAN_POINT('Ctrl Pts',(1.43309732687145,0.0123561690781439,
1.715480776583));
#20978=CARTESIAN_POINT('Ctrl Pts',(1.51213990150266,-0.093890993375447,
1.81902921434248));
#20979=CARTESIAN_POINT('Ctrl Pts',(1.57338902476662,-0.238090659850088,
1.90869858745619));
#20980=CARTESIAN_POINT('',(1.23077165948193,0.27609248605185,1.10727038327973));
#20981=CARTESIAN_POINT('Ctrl Pts',(1.23077165948193,0.27609248605185,1.10727038327973));
#20982=CARTESIAN_POINT('Ctrl Pts',(1.21397173814614,0.25604578597751,1.12805083925445));
#20983=CARTESIAN_POINT('Ctrl Pts',(1.19436482287741,0.235667011409686,1.15131250789252));
#20984=CARTESIAN_POINT('Ctrl Pts',(1.15844075168677,0.206554607000144,1.1919477734957));
#20985=CARTESIAN_POINT('Ctrl Pts',(1.14116749104432,0.19410271785776,1.2110848928));
#20986=CARTESIAN_POINT('Ctrl Pts',(1.10902103082114,0.178981360555533,1.24526606650682));
#20987=CARTESIAN_POINT('Ctrl Pts',(1.09145681862835,0.173166578774623,1.26352342884088));
#20988=CARTESIAN_POINT('Ctrl Pts',(1.06762054184321,0.171810769270086,1.28727233489076));
#20989=CARTESIAN_POINT('Ctrl Pts',(1.85754313061971,-0.153129647965883,
1.63615580822897));
#20990=CARTESIAN_POINT('Ctrl Pts',(1.81335940151627,-0.0607713534907822,
1.59083969670469));
#20991=CARTESIAN_POINT('Ctrl Pts',(1.75708539039456,0.0223614442500402,
1.54129005514746));
#20992=CARTESIAN_POINT('Ctrl Pts',(1.61733286423933,0.159600739735627,1.42521036359322));
#20993=CARTESIAN_POINT('Ctrl Pts',(1.53789592166465,0.208550308549111,1.36183966503053));
#20994=CARTESIAN_POINT('Ctrl Pts',(1.37907079095174,0.264206681902339,1.23219371736399));
#20995=CARTESIAN_POINT('Ctrl Pts',(1.30454791379682,0.275306576910198,1.17031259812848));
#20996=CARTESIAN_POINT('Ctrl Pts',(1.23077165948193,0.27609248605185,1.10727038327973));
#20997=CARTESIAN_POINT('Ctrl Pts',(1.06762054184321,0.171810769270086,1.28727233489076));
#20998=CARTESIAN_POINT('Ctrl Pts',(1.29491863831812,0.158856141562724,1.54044293163017));
#20999=CARTESIAN_POINT('Ctrl Pts',(1.46385147967852,0.0214114678431584,
1.74808806329354));
#21000=CARTESIAN_POINT('Ctrl Pts',(1.5744190659244,-0.240523251888611,1.91020772988088));
#21001=CARTESIAN_POINT('Ctrl Pts',(1.07192527046357,0.128593049303376,1.28727233489076));
#21002=CARTESIAN_POINT('Ctrl Pts',(1.2981540059198,0.106557157682628,1.54044293163017));
#21003=CARTESIAN_POINT('Ctrl Pts',(1.46116778184124,-0.0373276272898292,
1.74808806329354));
#21004=CARTESIAN_POINT('Ctrl Pts',(1.56096659822788,-0.303061305613996,
1.91020772988088));
#21005=CARTESIAN_POINT('Ctrl Pts',(1.07622999908393,0.0853753293366667,
1.28727233489076));
#21006=CARTESIAN_POINT('Ctrl Pts',(1.30138937352148,0.0542581738025322,
1.54044293163017));
#21007=CARTESIAN_POINT('Ctrl Pts',(1.45848408400396,-0.0960667224228172,
1.74808806329354));
#21008=CARTESIAN_POINT('Ctrl Pts',(1.54751413053135,-0.365599359339381,
1.91020772988088));
#21009=CARTESIAN_POINT('Ctrl Pts',(1.08053472770428,0.042157609369957,1.28727233489076));
#21010=CARTESIAN_POINT('Ctrl Pts',(1.30462474112317,0.00195918992243627,
1.54044293163017));
#21011=CARTESIAN_POINT('Ctrl Pts',(1.45580038616668,-0.154805817555805,
1.74808806329354));
#21012=CARTESIAN_POINT('Ctrl Pts',(1.53406166283483,-0.428137413064766,
1.91020772988088));
#21013=CARTESIAN_POINT('',(1.08053472770428,0.042157609369957,1.28727233489076));
#21014=CARTESIAN_POINT('Ctrl Pts',(1.08053472770428,0.042157609369957,1.28727233489076));
#21015=CARTESIAN_POINT('Ctrl Pts',(1.18019989616608,0.024279158719655,1.39987124007464));
#21016=CARTESIAN_POINT('Ctrl Pts',(1.26544208722232,-0.0166569869072256,
1.50346488650363));
#21017=CARTESIAN_POINT('Ctrl Pts',(1.42418037408903,-0.16009648734447,1.715480776583));
#21018=CARTESIAN_POINT('Ctrl Pts',(1.48987049850469,-0.275079075974333,
1.81902921434248));
#21019=CARTESIAN_POINT('Ctrl Pts',(1.53333167412,-0.425598593400271,1.90869858745619));
#21020=CARTESIAN_POINT('Ctrl Pts',(1.06762054184321,0.171810769270086,1.28727233489076));
#21021=CARTESIAN_POINT('Ctrl Pts',(1.0703931707,0.150205945126616,1.28796759655004));
#21022=CARTESIAN_POINT('Ctrl Pts',(1.07285457179227,0.128560761691046,1.2883190755065));
#21023=CARTESIAN_POINT('Ctrl Pts',(1.07501055311346,0.106874449528872,1.288319084765));
#21024=CARTESIAN_POINT('Ctrl Pts',(1.07715324084587,0.0853218532357679,
1.28831909396641));
#21025=CARTESIAN_POINT('Ctrl Pts',(1.07899214990168,0.0637502700203708,
1.28797193184368));
#21026=CARTESIAN_POINT('Ctrl Pts',(1.08053472770428,0.0421576093699569,
1.28727233489076));
#21027=CARTESIAN_POINT('Ctrl Pts',(1.07691421720911,0.0427958338937931,
1.28318517918604));
#21028=CARTESIAN_POINT('Ctrl Pts',(1.30237686203014,0.00374881610008822,
1.53750926858099));
#21029=CARTESIAN_POINT('Ctrl Pts',(1.45454290982716,-0.15247585021093,1.74606924121326));
#21030=CARTESIAN_POINT('Ctrl Pts',(1.53341236060018,-0.425878165039262,
1.90886509708284));
#21031=CARTESIAN_POINT('Ctrl Pts',(1.091545040475,0.0448924758011831,1.26845681306972));
#21032=CARTESIAN_POINT('Ctrl Pts',(1.32014932750452,0.0055908047641015,
1.51984840181958));
#21033=CARTESIAN_POINT('Ctrl Pts',(1.4745930125769,-0.152438895007652,1.72608377212012));
#21034=CARTESIAN_POINT('Ctrl Pts',(1.55488138991364,-0.429508274607607,
1.88700775532559));
#21035=CARTESIAN_POINT('Ctrl Pts',(1.11904054473513,0.0454099470705955,
1.24111941924412));
#21036=CARTESIAN_POINT('Ctrl Pts',(1.35337649424567,0.00503268467650712,
1.48709402322589));
#21037=CARTESIAN_POINT('Ctrl Pts',(1.51165038249934,-0.157175625948469,
1.68880469124906));
#21038=CARTESIAN_POINT('Ctrl Pts',(1.59385438982847,-0.441219201568131,
1.84625359892919));
#21039=CARTESIAN_POINT('Ctrl Pts',(1.18191630764681,0.026799925001142,1.18057686266081));
#21040=CARTESIAN_POINT('Ctrl Pts',(1.42860644524987,-0.0203022432084509,
1.41443159040039));
#21041=CARTESIAN_POINT('Ctrl Pts',(1.59265822923791,-0.19450578395595,1.60624053738541));
#21042=CARTESIAN_POINT('Ctrl Pts',(1.6740871562873,-0.495974904441967,1.75591502454111));
#21043=CARTESIAN_POINT('Ctrl Pts',(1.23181557314521,-0.00363238016698347,
1.1340877844534));
#21044=CARTESIAN_POINT('Ctrl Pts',(1.48747160844964,-0.0593232212680496,
1.35876508657128));
#21045=CARTESIAN_POINT('Ctrl Pts',(1.65371551508434,-0.245130498049609,
1.54303391436826));
#21046=CARTESIAN_POINT('Ctrl Pts',(1.73041945202572,-0.561310568731033,
1.68683916414419));
#21047=CARTESIAN_POINT('Ctrl Pts',(1.26719829440569,-0.0306796703370956,
1.10166698368801));
#21048=CARTESIAN_POINT('Ctrl Pts',(1.52894260490193,-0.0934843164788936,
1.3199705116299));
#21049=CARTESIAN_POINT('Ctrl Pts',(1.69583409006837,-0.288323673548516,
1.49898794576061));
#21050=CARTESIAN_POINT('Ctrl Pts',(1.76787274990501,-0.615197741545964,
1.63871928608014));
#21051=CARTESIAN_POINT('Ctrl Pts',(1.08053472770428,0.042157609369957,1.28727233489076));
#21052=CARTESIAN_POINT('Ctrl Pts',(1.1129292020849,0.0467681993550386,1.25472274024223));
#21053=CARTESIAN_POINT('Ctrl Pts',(1.13992065666396,0.0416051146519737,
1.22803799031325));
#21054=CARTESIAN_POINT('Ctrl Pts',(1.19777852863138,0.016827672483465,1.1707920398715));
#21055=CARTESIAN_POINT('Ctrl Pts',(1.22835394451345,-0.000751694447614519,
1.14052203161171));
#21056=CARTESIAN_POINT('Ctrl Pts',(1.26108935601086,-0.026068655399315,
1.10727038327973));
#21057=CARTESIAN_POINT('Origin',(0.,0.,1.38794976669063));
#21058=CARTESIAN_POINT('',(-0.7,-8.57252759403147E-17,1.66862915010152));
#21059=CARTESIAN_POINT('Origin',(0.,0.,1.66862915010152));
#21060=CARTESIAN_POINT('',(-0.980679383410898,-1.20098586788396E-16,1.38794976669063));
#21061=CARTESIAN_POINT('Origin',(0.,0.,1.10727038327973));
#21062=CARTESIAN_POINT('Origin',(0.,0.,1.37171309575435));
#21063=CARTESIAN_POINT('Origin',(0.541,0.,2.6));
#21064=CARTESIAN_POINT('',(-0.541,-6.62533918338718E-17,2.6));
#21065=CARTESIAN_POINT('Origin',(0.,0.,2.6));
#21066=CARTESIAN_POINT('Origin',(0.,0.,2.58));
#21067=CARTESIAN_POINT('',(-0.501,-6.13548046372824E-17,2.56));
#21068=CARTESIAN_POINT('',(-0.521,-6.38040982355771E-17,2.58));
#21069=CARTESIAN_POINT('Origin',(0.,0.,2.56));
#21070=CARTESIAN_POINT('Origin',(0.,0.,2.13431457505076));
#21071=CARTESIAN_POINT('',(-0.501,-6.13548046372824E-17,1.70862915010152));
#21072=CARTESIAN_POINT('',(-0.501,-6.13548046372824E-17,2.13431457505076));
#21073=CARTESIAN_POINT('Origin',(0.,0.,1.70862915010152));
#21074=CARTESIAN_POINT('Origin',(0.,0.,1.68862915010152));
#21075=CARTESIAN_POINT('',(-0.541,-6.62533918338718E-17,1.66862915010152));
#21076=CARTESIAN_POINT('',(-0.521,-6.38040982355771E-17,1.68862915010152));
#21077=CARTESIAN_POINT('Origin',(0.,0.,1.66862915010152));
#21078=CARTESIAN_POINT('Origin',(0.7,0.,1.66862915010152));
#21079=CARTESIAN_POINT('',(0.,0.,0.));
#21080=CARTESIAN_POINT('Origin',(0.,0.,10.98));
#21081=CARTESIAN_POINT('',(0.14,1.71450551880629E-17,11.));
#21082=CARTESIAN_POINT('Origin',(0.,0.,11.));
#21083=CARTESIAN_POINT('',(0.1,-1.22464679914735E-17,10.96));
#21084=CARTESIAN_POINT('',(0.12,1.46957615897682E-17,10.98));
#21085=CARTESIAN_POINT('',(-0.1,-1.22464679914735E-17,10.96));
#21086=CARTESIAN_POINT('Origin',(0.,0.,10.96));
#21087=CARTESIAN_POINT('Origin',(0.,0.,10.96));
#21088=CARTESIAN_POINT('Origin',(0.,0.,10.875));
#21089=CARTESIAN_POINT('',(-0.1,-1.22464679914735E-17,10.75));
#21090=CARTESIAN_POINT('Origin',(0.,0.,10.75));
#21091=CARTESIAN_POINT('',(-0.1,-1.22464679914735E-17,10.875));
#21092=CARTESIAN_POINT('Origin',(0.,0.,11.));
#21093=CARTESIAN_POINT('',(-0.45,-5.51091059616309E-17,11.));
#21094=CARTESIAN_POINT('Origin',(0.,0.,11.));
#21095=CARTESIAN_POINT('Origin',(0.,0.,10.72));
#21096=CARTESIAN_POINT('',(0.,0.,10.69));
#21097=CARTESIAN_POINT('',(-0.05,-6.12323399573677E-18,10.72));
#21098=CARTESIAN_POINT('Origin',(0.,0.6,2.75));
#21099=CARTESIAN_POINT('',(0.217944947177034,0.45,2.75));
#21100=CARTESIAN_POINT('',(-0.217944947177034,0.45,2.75));
#21101=CARTESIAN_POINT('Origin',(0.,0.,2.75));
#21102=CARTESIAN_POINT('',(0.,0.45,2.75));
#21103=CARTESIAN_POINT('Origin',(0.,0.45,1.95));
#21104=CARTESIAN_POINT('',(-0.217944947177034,0.45,1.95));
#21105=CARTESIAN_POINT('',(0.217944947177034,0.45,1.95));
#21106=CARTESIAN_POINT('Origin',(0.,0.,1.95));
#21107=CARTESIAN_POINT('',(0.,0.45,1.95));
#21108=CARTESIAN_POINT('Origin',(0.,0.45,2.75));
#21109=CARTESIAN_POINT('',(0.217944947177034,0.45,3.76));
#21110=CARTESIAN_POINT('',(-0.217944947177034,0.45,3.76));
#21111=CARTESIAN_POINT('Origin',(0.6,0.,1.95));
#21112=CARTESIAN_POINT('',(0.45,0.217944947177034,1.95));
#21113=CARTESIAN_POINT('',(0.45,-0.217944947177034,1.95));
#21114=CARTESIAN_POINT('Origin',(0.,0.,1.95));
#21115=CARTESIAN_POINT('',(0.45,0.,1.95));
#21116=CARTESIAN_POINT('Origin',(0.45,0.,1.95));
#21117=CARTESIAN_POINT('',(0.45,0.217944947177034,2.75));
#21118=CARTESIAN_POINT('',(0.45,0.217944947177034,3.76));
#21119=CARTESIAN_POINT('',(0.45,-0.217944947177034,2.75));
#21120=CARTESIAN_POINT('',(0.45,0.,2.75));
#21121=CARTESIAN_POINT('',(0.45,-0.217944947177034,3.76));
#21122=CARTESIAN_POINT('Origin',(0.45,0.,2.75));
#21123=CARTESIAN_POINT('Origin',(0.,0.,2.75));
#21124=CARTESIAN_POINT('Origin',(0.45,0.,1.72));
#21125=CARTESIAN_POINT('',(-0.45,-5.51091059616309E-17,1.72));
#21126=CARTESIAN_POINT('Origin',(0.,0.,1.72));
#21127=CARTESIAN_POINT('Origin',(0.,0.,1.745));
#21128=CARTESIAN_POINT('',(-0.499999999999999,-6.12323399573676E-17,1.77));
#21129=CARTESIAN_POINT('Origin',(0.,0.,1.77));
#21130=CARTESIAN_POINT('',(-0.475,-5.81707229594993E-17,1.745));
#21131=CARTESIAN_POINT('Origin',(0.,0.,3.76));
#21132=CARTESIAN_POINT('',(-0.5,-6.12323399573677E-17,5.75));
#21133=CARTESIAN_POINT('Origin',(0.,0.,5.75));
#21134=CARTESIAN_POINT('',(-0.5,-6.12323399573677E-17,3.76));
#21135=CARTESIAN_POINT('Origin',(0.48,0.,5.75));
#21136=CARTESIAN_POINT('',(-0.48,-5.87830463590729E-17,5.75));
#21137=CARTESIAN_POINT('Origin',(0.,0.,5.75));
#21138=CARTESIAN_POINT('Origin',(0.,0.,5.805));
#21139=CARTESIAN_POINT('',(-0.48,-5.87830463590729E-17,5.86));
#21140=CARTESIAN_POINT('Origin',(0.,0.,5.86));
#21141=CARTESIAN_POINT('',(-0.48,-5.87830463590729E-17,5.805));
#21142=CARTESIAN_POINT('Origin',(0.5,0.,5.86));
#21143=CARTESIAN_POINT('',(-0.5,-6.12323399573677E-17,5.86));
#21144=CARTESIAN_POINT('Origin',(0.,0.,5.86));
#21145=CARTESIAN_POINT('Origin',(0.,0.,8.405));
#21146=CARTESIAN_POINT('',(-0.5,-6.12323399573677E-17,10.95));
#21147=CARTESIAN_POINT('Origin',(0.,0.,10.95));
#21148=CARTESIAN_POINT('',(-0.5,-6.12323399573677E-17,8.405));
#21149=CARTESIAN_POINT('Origin',(0.,0.,10.975));
#21150=CARTESIAN_POINT('',(-0.475,-5.81707229594993E-17,10.975));
#21151=CARTESIAN_POINT('',(0.,0.,0.));
#21152=CARTESIAN_POINT('Ctrl Pts',(0.999999999998244,-1.87406103457374E-6,
2.60499999999311));
#21153=CARTESIAN_POINT('Ctrl Pts',(1.00000006288704,0.033555619638003,2.60500024661583));
#21154=CARTESIAN_POINT('Ctrl Pts',(0.996432788538549,0.100793877077062,
2.59172126532562));
#21155=CARTESIAN_POINT('Ctrl Pts',(0.987779661769916,0.157562252712982,
2.55296011060328));
#21156=CARTESIAN_POINT('Ctrl Pts',(0.977968286593196,0.211192459212548,
2.49909481560466));
#21157=CARTESIAN_POINT('Ctrl Pts',(0.970281147530057,0.242238373929747,
2.44471009644067));
#21158=CARTESIAN_POINT('Ctrl Pts',(0.967388261055284,0.253317392831602,
2.37452193295668));
#21159=CARTESIAN_POINT('Ctrl Pts',(0.967116369990459,0.254356366300813,
2.34056467313598));
#21160=CARTESIAN_POINT('Ctrl Pts',(0.968060909182331,0.250746912814477,
2.30584393595531));
#21161=CARTESIAN_POINT('Ctrl Pts',(0.971275486994325,0.238235555290696,
2.25382796860057));
#21162=CARTESIAN_POINT('Ctrl Pts',(0.978160761261309,0.209370469448592,
2.20003517000389));
#21163=CARTESIAN_POINT('Ctrl Pts',(0.986928061083623,0.163194558725017,
2.1514224394046));
#21164=CARTESIAN_POINT('Ctrl Pts',(0.994800163464163,0.109016749833536,
2.11560611365411));
#21165=CARTESIAN_POINT('Ctrl Pts',(1.00003726905853,0.0393234864952561,
2.09484257852823));
#21166=CARTESIAN_POINT('Ctrl Pts',(1.00039359739908,-0.0285679116079913,
2.09347899005165));
#21167=CARTESIAN_POINT('Ctrl Pts',(0.995946129986918,-0.098499816085455,
2.11089539860567));
#21168=CARTESIAN_POINT('Ctrl Pts',(0.987595534630939,-0.160108842507484,
2.14787016428115));
#21169=CARTESIAN_POINT('Ctrl Pts',(0.978767296657426,-0.20640426202618,
2.19598850651528));
#21170=CARTESIAN_POINT('Ctrl Pts',(0.97062172581105,-0.241091125419321,
2.25963518301816));
#21171=CARTESIAN_POINT('Ctrl Pts',(0.967038345237899,-0.254607790735269,
2.32400532558939));
#21172=CARTESIAN_POINT('Ctrl Pts',(0.967372392238064,-0.253367892292085,
2.39214155711082));
#21173=CARTESIAN_POINT('Ctrl Pts',(0.971848592631414,-0.236216524025834,
2.45101723423612));
#21174=CARTESIAN_POINT('Ctrl Pts',(0.977999994055034,-0.208938409888944,
2.49656599568729));
#21175=CARTESIAN_POINT('Ctrl Pts',(0.982365078241419,-0.187417224408925,
2.52354132496555));
#21176=CARTESIAN_POINT('Ctrl Pts',(0.986694720178997,-0.163267539196543,
2.54663242388917));
#21177=CARTESIAN_POINT('Ctrl Pts',(0.99244571253526,-0.125541882265517,
2.57418619605903));
#21178=CARTESIAN_POINT('Ctrl Pts',(0.998300344088637,-0.0706101566680352,
2.59849422048893));
#21179=CARTESIAN_POINT('Ctrl Pts',(0.999999955756101,-0.0236095057558304,
2.60499982649452));
#21180=CARTESIAN_POINT('Ctrl Pts',(0.999999999998244,-1.87406103457374E-6,
2.60499999999311));
#21181=CARTESIAN_POINT('Ctrl Pts',(0.983333333331803,-1.72646341714646E-6,
2.58833333332708));
#21182=CARTESIAN_POINT('Ctrl Pts',(0.983325070408895,0.0309254949332375,
2.58831701644367));
#21183=CARTESIAN_POINT('Ctrl Pts',(0.980235431771385,0.0928701985922922,
2.5763334457126));
#21184=CARTESIAN_POINT('Ctrl Pts',(0.97262951086769,0.146010496479255,2.54070549738907));
#21185=CARTESIAN_POINT('Ctrl Pts',(0.963966193226361,0.196619990384259,
2.49071684326285));
#21186=CARTESIAN_POINT('Ctrl Pts',(0.957121635980358,0.226408216243534,
2.43967803502293));
#21187=CARTESIAN_POINT('Ctrl Pts',(0.954530758590317,0.237116103160976,
2.37322988185745));
#21188=CARTESIAN_POINT('Ctrl Pts',(0.954292056495262,0.238108034056394,
2.34106055897148));
#21189=CARTESIAN_POINT('Ctrl Pts',(0.955131698824161,0.234634460337268,
2.30818704053657));
#21190=CARTESIAN_POINT('Ctrl Pts',(0.958005717805603,0.222572733944937,
2.2590085409333));
#21191=CARTESIAN_POINT('Ctrl Pts',(0.964133168526514,0.194921019608955,
2.20849850875947));
#21192=CARTESIAN_POINT('Ctrl Pts',(0.971886775166395,0.151277899039362,
2.16333241887712));
#21193=CARTESIAN_POINT('Ctrl Pts',(0.978798486508062,0.100613721566294,
2.13040797264567));
#21194=CARTESIAN_POINT('Ctrl Pts',(0.983369400970407,0.0361963313628681,
2.11151394416968));
#21195=CARTESIAN_POINT('Ctrl Pts',(0.983676824334791,-0.0262950908417384,
2.11028422573118));
#21196=CARTESIAN_POINT('Ctrl Pts',(0.979801092832465,-0.0908603189323969,
2.12610656815928));
#21197=CARTESIAN_POINT('Ctrl Pts',(0.972473802924845,-0.148358154753562,
2.16004581981554));
#21198=CARTESIAN_POINT('Ctrl Pts',(0.964672149439096,-0.192110727398231,
2.20471275196644));
#21199=CARTESIAN_POINT('Ctrl Pts',(0.957427193110245,-0.225297504050057,
2.26446164543395));
#21200=CARTESIAN_POINT('Ctrl Pts',(0.954222830159563,-0.238355411074918,
2.32536038420973));
#21201=CARTESIAN_POINT('Ctrl Pts',(0.954522079095343,-0.2371523061421,2.3899277120541));
#21202=CARTESIAN_POINT('Ctrl Pts',(0.958517953243843,-0.220614507903057,
2.4455635357429));
#21203=CARTESIAN_POINT('Ctrl Pts',(0.963982071416956,-0.194581079725971,
2.48825477624319));
#21204=CARTESIAN_POINT('Ctrl Pts',(0.967849868185066,-0.174169675975904,
2.51340938027297));
#21205=CARTESIAN_POINT('Ctrl Pts',(0.97167321111088,-0.151401045973518,
2.53482806141593));
#21206=CARTESIAN_POINT('Ctrl Pts',(0.976733295652627,-0.116052309467583,
2.56023494607926));
#21207=CARTESIAN_POINT('Ctrl Pts',(0.981853837292877,-0.0650450913579237,
2.58243716495324));
#21208=CARTESIAN_POINT('Ctrl Pts',(0.983332905880957,-0.0217501188318965,
2.58833203941799));
#21209=CARTESIAN_POINT('Ctrl Pts',(0.983333333331803,-1.72646341714646E-6,
2.58833333332708));
#21210=CARTESIAN_POINT('Ctrl Pts',(0.966666666665363,-1.57886579971917E-6,
2.57166666666104));
#21211=CARTESIAN_POINT('Ctrl Pts',(0.966675031089233,0.0282574067618839,
2.57168340910161));
#21212=CARTESIAN_POINT('Ctrl Pts',(0.964030995123869,0.0849671350523733,
2.56092437077672));
#21213=CARTESIAN_POINT('Ctrl Pts',(0.957496079669552,0.134432741424285,
2.52848314020048));
#21214=CARTESIAN_POINT('Ctrl Pts',(0.949965488618089,0.18202293386404,2.48231761863255));
#21215=CARTESIAN_POINT('Ctrl Pts',(0.943960096058651,0.210589600813346,
2.4346289274524));
#21216=CARTESIAN_POINT('Ctrl Pts',(0.941686431722323,0.220882428486858,
2.3719223211333));
#21217=CARTESIAN_POINT('Ctrl Pts',(0.94146963989202,0.221854615130021,2.34155719007975));
#21218=CARTESIAN_POINT('Ctrl Pts',(0.942215861234142,0.218493014540143,
2.31051805593517));
#21219=CARTESIAN_POINT('Ctrl Pts',(0.944737453851974,0.206900615314252,
2.26419080172698));
#21220=CARTESIAN_POINT('Ctrl Pts',(0.950105713610565,0.180489574889026,
2.21697132240232));
#21221=CARTESIAN_POINT('Ctrl Pts',(0.956837948144641,0.139371349739201,
2.17526823220057));
#21222=CARTESIAN_POINT('Ctrl Pts',(0.962797300252717,0.0922406494407946,
2.14521214199563));
#21223=CARTESIAN_POINT('Ctrl Pts',(0.966692768725039,0.0330593334366949,
2.12821013824094));
#21224=CARTESIAN_POINT('Ctrl Pts',(0.966958180635997,-0.0240006511464648,
2.12709572724774));
#21225=CARTESIAN_POINT('Ctrl Pts',(0.963654605188848,-0.08321040561347,
2.1413234011611));
#21226=CARTESIAN_POINT('Ctrl Pts',(0.957353720921044,-0.136587098613656,
2.17220985324203));
#21227=CARTESIAN_POINT('Ctrl Pts',(0.950573235959199,-0.177820331414012,
2.21345060010943));
#21228=CARTESIAN_POINT('Ctrl Pts',(0.944223169736954,-0.209514123317684,
2.26930212368042));
#21229=CARTESIAN_POINT('Ctrl Pts',(0.941403959395846,-0.222103494504004,
2.32673583609555));
#21230=CARTESIAN_POINT('Ctrl Pts',(0.941667556372663,-0.220946133881027,
2.38772812706794));
#21231=CARTESIAN_POINT('Ctrl Pts',(0.945187704752525,-0.205008502652309,
2.44011245850097));
#21232=CARTESIAN_POINT('Ctrl Pts',(0.94997031235299,-0.180221173921234,
2.47994404421443));
#21233=CARTESIAN_POINT('Ctrl Pts',(0.953336718390379,-0.160920110206714,
2.5032802399603));
#21234=CARTESIAN_POINT('Ctrl Pts',(0.956651963018509,-0.139538170190601,
2.5230099883211));
#21235=CARTESIAN_POINT('Ctrl Pts',(0.961021973375283,-0.10656485199273,
2.54628159282629));
#21236=CARTESIAN_POINT('Ctrl Pts',(0.965409168116845,-0.0594989402485911,
2.56637680898634));
#21237=CARTESIAN_POINT('Ctrl Pts',(0.966667022710479,-0.0198905682807695,
2.57166766119149));
#21238=CARTESIAN_POINT('Ctrl Pts',(0.966666666665363,-1.57886579971917E-6,
2.57166666666104));
#21239=CARTESIAN_POINT('Ctrl Pts',(0.949999999998922,-1.43126818229188E-6,
2.554999999995));
#21240=CARTESIAN_POINT('Ctrl Pts',(0.950000038611092,0.0256272820571184,
2.55500017892945));
#21241=CARTESIAN_POINT('Ctrl Pts',(0.947833638356706,0.077043456567603,
2.5455365511637));
#21242=CARTESIAN_POINT('Ctrl Pts',(0.942345928767326,0.122880985190557,
2.51622852698627));
#21243=CARTESIAN_POINT('Ctrl Pts',(0.935963395251255,0.167450465035751,
2.47393964629074));
#21244=CARTESIAN_POINT('Ctrl Pts',(0.930800584508952,0.194759443127133,
2.42959686603466));
#21245=CARTESIAN_POINT('Ctrl Pts',(0.928828929257356,0.204681138816232,
2.37063027003408));
#21246=CARTESIAN_POINT('Ctrl Pts',(0.928645326396822,0.205606282885602,
2.34205307591525));
#21247=CARTESIAN_POINT('Ctrl Pts',(0.929286650875972,0.202380562062934,
2.31286116051643));
#21248=CARTESIAN_POINT('Ctrl Pts',(0.931467684663253,0.191237793968494,
2.26937137405972));
#21249=CARTESIAN_POINT('Ctrl Pts',(0.93607812087577,0.166040125049389,2.2254346611579));
#21250=CARTESIAN_POINT('Ctrl Pts',(0.941796662227414,0.127454690053546,
2.18717821167308));
#21251=CARTESIAN_POINT('Ctrl Pts',(0.946795623296616,0.0838376211735529,
2.16001400098719));
#21252=CARTESIAN_POINT('Ctrl Pts',(0.950024900636915,0.0299321783043069,
2.14488150388239));
#21253=CARTESIAN_POINT('Ctrl Pts',(0.950241407571709,-0.0217278303802119,
2.14390096292727));
#21254=CARTESIAN_POINT('Ctrl Pts',(0.947509568034395,-0.0755709084604119,
2.15653457071471));
#21255=CARTESIAN_POINT('Ctrl Pts',(0.942231989214949,-0.124836410859733,
2.18438550877642));
#21256=CARTESIAN_POINT('Ctrl Pts',(0.936478088740869,-0.163526796786063,
2.22217484556059));
#21257=CARTESIAN_POINT('Ctrl Pts',(0.931028637036149,-0.19372050194842,
2.27412858609622));
#21258=CARTESIAN_POINT('Ctrl Pts',(0.92858844431751,-0.205851114843653,
2.32809089471589));
#21259=CARTESIAN_POINT('Ctrl Pts',(0.928817243229942,-0.204730547731042,
2.38551428201123));
#21260=CARTESIAN_POINT('Ctrl Pts',(0.931857065364954,-0.189406486529532,
2.43465876000775));
#21261=CARTESIAN_POINT('Ctrl Pts',(0.935952389714912,-0.165863843758261,
2.47163282477033));
#21262=CARTESIAN_POINT('Ctrl Pts',(0.938821508334025,-0.147672561773693,
2.49314829526772));
#21263=CARTESIAN_POINT('Ctrl Pts',(0.941630453950392,-0.127671676967576,
2.51120562584786));
#21264=CARTESIAN_POINT('Ctrl Pts',(0.945309556492649,-0.0970752791947962,
2.53233034284651));
#21265=CARTESIAN_POINT('Ctrl Pts',(0.948962661321086,-0.0539338749384796,
2.55031975345065));
#21266=CARTESIAN_POINT('Ctrl Pts',(0.949999972835335,-0.0180311813568356,
2.55499987411497));
#21267=CARTESIAN_POINT('Ctrl Pts',(0.949999999998922,-1.43126818229188E-6,
2.554999999995));
#21268=CARTESIAN_POINT('',(0.998737211088938,0.0502392594122345,2.10000000017302));
#21269=CARTESIAN_POINT('',(0.998737211088938,-0.0502392594122345,2.10000000017302));
#21270=CARTESIAN_POINT('Ctrl Pts',(0.998741489349531,0.0501276226578845,
2.09998790761528));
#21271=CARTESIAN_POINT('Ctrl Pts',(0.998209106442774,0.0465065804968853,
2.0999823604152));
#21272=CARTESIAN_POINT('Ctrl Pts',(0.997731917482903,0.0428858888083561,
2.09997532142456));
#21273=CARTESIAN_POINT('Ctrl Pts',(0.99731100353809,0.0392650986878338,
2.09996763820277));
#21274=CARTESIAN_POINT('Ctrl Pts',(0.996973673612343,0.0363633158470504,
2.0999614806956));
#21275=CARTESIAN_POINT('Ctrl Pts',(0.996672480569791,0.0334615115052595,
2.09995491761494));
#21276=CARTESIAN_POINT('Ctrl Pts',(0.996408345014525,0.0305539602702526,
2.09994817558028));
#21277=CARTESIAN_POINT('Ctrl Pts',(0.995823734577335,0.0241186857880212,
2.09993325345505));
#21278=CARTESIAN_POINT('Ctrl Pts',(0.995422878237189,0.0176782325627147,
2.09991691990568));
#21279=CARTESIAN_POINT('Ctrl Pts',(0.995209369745946,0.0111608079949593,
2.0999080411453));
#21280=CARTESIAN_POINT('Ctrl Pts',(0.99514171218205,0.00909553618039141,
2.09990522760241));
#21281=CARTESIAN_POINT('Ctrl Pts',(0.995092895768509,0.00702412914613266,
2.09990323613576));
#21282=CARTESIAN_POINT('Ctrl Pts',(0.99506286554661,0.00494410069252508,
2.0999025509242));
#21283=CARTESIAN_POINT('Ctrl Pts',(0.99504459933955,0.00367890090298719,
2.09990213413686));
#21284=CARTESIAN_POINT('Ctrl Pts',(0.995033286585864,0.00241076308799952,
2.09990220272711));
#21285=CARTESIAN_POINT('Ctrl Pts',(0.995028899524127,0.00113911783449072,
2.09990288388685));
#21286=CARTESIAN_POINT('Ctrl Pts',(0.995024963884268,-1.67708640180092E-6,
2.09990349495629));
#21287=CARTESIAN_POINT('Ctrl Pts',(0.995026593989671,-0.00114513314823198,
2.09990463268876));
#21288=CARTESIAN_POINT('Ctrl Pts',(0.995033805529301,-0.00228459200009584,
2.09990622411078));
#21289=CARTESIAN_POINT('Ctrl Pts',(0.995042806799174,-0.00370683706316931,
2.09990821048536));
#21290=CARTESIAN_POINT('Ctrl Pts',(0.995060508292759,-0.00512536873273449,
2.09991087886862));
#21291=CARTESIAN_POINT('Ctrl Pts',(0.99508694937675,-0.00654097371496716,
2.0999140064208));
#21292=CARTESIAN_POINT('Ctrl Pts',(0.995138761674284,-0.00931490486528927,
2.09992013497682));
#21293=CARTESIAN_POINT('Ctrl Pts',(0.995224111395307,-0.0120760964135134,
2.09992800145899));
#21294=CARTESIAN_POINT('Ctrl Pts',(0.995343089287915,-0.0148303143798948,
2.09993619328405));
#21295=CARTESIAN_POINT('Ctrl Pts',(0.995539967164857,-0.0193878382523947,
2.09994974865211));
#21296=CARTESIAN_POINT('Ctrl Pts',(0.995828617967945,-0.0239182715715797,
2.09996404004403));
#21297=CARTESIAN_POINT('Ctrl Pts',(0.996207735735797,-0.0284458173699921,
2.09997472302851));
#21298=CARTESIAN_POINT('Ctrl Pts',(0.99631850279087,-0.0297686330154764,
2.09997784428219));
#21299=CARTESIAN_POINT('Ctrl Pts',(0.996436986832906,-0.0310911807891784,
2.09998067371155));
#21300=CARTESIAN_POINT('Ctrl Pts',(0.996563166797704,-0.0324135784390754,
2.09998318511707));
#21301=CARTESIAN_POINT('Ctrl Pts',(0.997133221361869,-0.0383878931186965,
2.09999453111945));
#21302=CARTESIAN_POINT('Ctrl Pts',(0.997858925779834,-0.0443424598651534,
2.09999902027607));
#21303=CARTESIAN_POINT('Ctrl Pts',(0.998734041876947,-0.0502864563072932,
2.0999972397247));
#21304=CARTESIAN_POINT('',(0.987458837468112,0.157876674357314,2.54999999999916));
#21305=CARTESIAN_POINT('Ctrl Pts',(0.998741489263531,0.0501276243402692,
2.09998790795724));
#21306=CARTESIAN_POINT('Ctrl Pts',(0.997746174412029,0.0695985876399753,
2.10394554683626));
#21307=CARTESIAN_POINT('Ctrl Pts',(0.994363645806935,0.112020975270126,
2.11759217250489));
#21308=CARTESIAN_POINT('Ctrl Pts',(0.986928061083623,0.163194558725017,
2.1514224394046));
#21309=CARTESIAN_POINT('Ctrl Pts',(0.978160761261309,0.209370469448592,
2.20003517000389));
#21310=CARTESIAN_POINT('Ctrl Pts',(0.971275486994325,0.238235555290696,
2.25382796860057));
#21311=CARTESIAN_POINT('Ctrl Pts',(0.968060909182331,0.250746912814477,
2.30584393595531));
#21312=CARTESIAN_POINT('Ctrl Pts',(0.967116369990459,0.254356366300813,
2.34056467313598));
#21313=CARTESIAN_POINT('Ctrl Pts',(0.967388261055284,0.253317392831602,
2.37452193295668));
#21314=CARTESIAN_POINT('Ctrl Pts',(0.970281147530057,0.242238373929747,
2.44471009644067));
#21315=CARTESIAN_POINT('Ctrl Pts',(0.977968286593196,0.211192459212548,
2.49909481560466));
#21316=CARTESIAN_POINT('Ctrl Pts',(0.98494013308223,0.173083472433883,2.53737085347425));
#21317=CARTESIAN_POINT('Ctrl Pts',(0.986199840262143,0.165761961406214,
2.54388428246999));
#21318=CARTESIAN_POINT('Ctrl Pts',(0.987440095705288,0.157976027584706,
2.55002758371622));
#21319=CARTESIAN_POINT('',(0.972500000001548,-1.63052496584468E-6,2.57749999999709));
#21320=CARTESIAN_POINT('Ctrl Pts',(0.987458837468451,0.157876674355192,
2.55));
#21321=CARTESIAN_POINT('Ctrl Pts',(0.985294697406766,0.146794280964263,
2.55388665064189));
#21322=CARTESIAN_POINT('Ctrl Pts',(0.983354421647032,0.135549889588831,
2.55740912752908));
#21323=CARTESIAN_POINT('Ctrl Pts',(0.977055328631449,0.0935709003424381,
2.56892572544489));
#21324=CARTESIAN_POINT('Ctrl Pts',(0.974161715360584,0.0622013742464855,
2.57437596695135));
#21325=CARTESIAN_POINT('Ctrl Pts',(0.972834706545006,0.0246194032981655,
2.57687004873351));
#21326=CARTESIAN_POINT('Ctrl Pts',(0.972691422895011,0.0189840464089377,
2.57713968402705));
#21327=CARTESIAN_POINT('Ctrl Pts',(0.972559701868467,0.0105124985263587,
2.57738760007473));
#21328=CARTESIAN_POINT('Ctrl Pts',(0.972529696233088,0.0076814295447408,
2.5774440907214));
#21329=CARTESIAN_POINT('Ctrl Pts',(0.972504563213093,0.00323267114025078,
2.57749140831944));
#21330=CARTESIAN_POINT('Ctrl Pts',(0.972499996930093,0.00161553516506767,
2.57750000577993));
#21331=CARTESIAN_POINT('Ctrl Pts',(0.972500000001548,-1.63052496584468E-6,
2.57749999999708));
#21332=CARTESIAN_POINT('',(0.949999999998922,-1.43126818229188E-6,2.554999999995));
#21333=CARTESIAN_POINT('Ctrl Pts',(0.972500000001548,-1.63052496584468E-6,
2.57749999999709));
#21334=CARTESIAN_POINT('Ctrl Pts',(0.965000000000673,-1.56410603799375E-6,
2.56999999999639));
#21335=CARTESIAN_POINT('Ctrl Pts',(0.957499999999797,-1.49768711014282E-6,
2.5624999999957));
#21336=CARTESIAN_POINT('Ctrl Pts',(0.949999999998922,-1.43126818229188E-6,
2.554999999995));
#21337=CARTESIAN_POINT('',(0.950017413548361,2.77722566314428E-6,2.14493017758226));
#21338=CARTESIAN_POINT('Ctrl Pts',(0.949999999998922,-1.43126818229188E-6,
2.554999999995));
#21339=CARTESIAN_POINT('Ctrl Pts',(0.950000038611092,0.0256272820571184,
2.55500017892945));
#21340=CARTESIAN_POINT('Ctrl Pts',(0.947833638356706,0.077043456567603,
2.5455365511637));
#21341=CARTESIAN_POINT('Ctrl Pts',(0.942345928767326,0.122880985190557,
2.51622852698627));
#21342=CARTESIAN_POINT('Ctrl Pts',(0.935963395251255,0.167450465035751,
2.47393964629074));
#21343=CARTESIAN_POINT('Ctrl Pts',(0.930800584508952,0.194759443127133,
2.42959686603466));
#21344=CARTESIAN_POINT('Ctrl Pts',(0.928828929257356,0.204681138816232,
2.37063027003408));
#21345=CARTESIAN_POINT('Ctrl Pts',(0.928645326396822,0.205606282885602,
2.34205307591525));
#21346=CARTESIAN_POINT('Ctrl Pts',(0.929286650875972,0.202380562062934,
2.31286116051643));
#21347=CARTESIAN_POINT('Ctrl Pts',(0.931467684663253,0.191237793968494,
2.26937137405972));
#21348=CARTESIAN_POINT('Ctrl Pts',(0.93607812087577,0.166040125049389,2.2254346611579));
#21349=CARTESIAN_POINT('Ctrl Pts',(0.941796662227414,0.127454690053546,
2.18717821167308));
#21350=CARTESIAN_POINT('Ctrl Pts',(0.946795623296616,0.0838376211735529,
2.16001400098719));
#21351=CARTESIAN_POINT('Ctrl Pts',(0.949571221584807,0.0375053185605399,
2.14700745845955));
#21352=CARTESIAN_POINT('Ctrl Pts',(0.950019209030419,0.0100740119424525,
2.1449223021834));
#21353=CARTESIAN_POINT('Ctrl Pts',(0.950017413548361,2.77722566314337E-6,
2.14493017758226));
#21354=CARTESIAN_POINT('Ctrl Pts',(0.950017413548361,2.77722566314337E-6,
2.14493017758226));
#21355=CARTESIAN_POINT('Ctrl Pts',(0.950016105516441,-0.0073342476264757,
2.14493591491227));
#21356=CARTESIAN_POINT('Ctrl Pts',(0.949714588734556,-0.0321111444056223,
2.14633727826451));
#21357=CARTESIAN_POINT('Ctrl Pts',(0.947509568034395,-0.0755709084604119,
2.15653457071471));
#21358=CARTESIAN_POINT('Ctrl Pts',(0.942231989214949,-0.124836410859733,
2.18438550877642));
#21359=CARTESIAN_POINT('Ctrl Pts',(0.936478088740869,-0.163526796786063,
2.22217484556059));
#21360=CARTESIAN_POINT('Ctrl Pts',(0.931028637036149,-0.19372050194842,
2.27412858609622));
#21361=CARTESIAN_POINT('Ctrl Pts',(0.92858844431751,-0.205851114843653,
2.32809089471589));
#21362=CARTESIAN_POINT('Ctrl Pts',(0.928817243229942,-0.204730547731042,
2.38551428201123));
#21363=CARTESIAN_POINT('Ctrl Pts',(0.931857065364954,-0.189406486529532,
2.43465876000775));
#21364=CARTESIAN_POINT('Ctrl Pts',(0.935952389714912,-0.165863843758261,
2.47163282477033));
#21365=CARTESIAN_POINT('Ctrl Pts',(0.938821508334025,-0.147672561773693,
2.49314829526772));
#21366=CARTESIAN_POINT('Ctrl Pts',(0.941630453950392,-0.127671676967576,
2.51120562584786));
#21367=CARTESIAN_POINT('Ctrl Pts',(0.945309556492649,-0.0970752791947962,
2.53233034284651));
#21368=CARTESIAN_POINT('Ctrl Pts',(0.948962661321086,-0.0539338749384796,
2.55031975345065));
#21369=CARTESIAN_POINT('Ctrl Pts',(0.949999972835335,-0.0180311813568356,
2.55499987411497));
#21370=CARTESIAN_POINT('Ctrl Pts',(0.949999999998922,-1.43126818229188E-6,
2.554999999995));
#21371=CARTESIAN_POINT('',(0.987458837468112,-0.157876674357314,2.54999999999916));
#21372=CARTESIAN_POINT('Ctrl Pts',(0.972500000001548,-1.63052496584468E-6,
2.57749999999708));
#21373=CARTESIAN_POINT('Ctrl Pts',(0.972500001100936,-0.00058047386256792,
2.57749999792719));
#21374=CARTESIAN_POINT('Ctrl Pts',(0.972500587629742,-0.00115932100720252,
2.5774988936244));
#21375=CARTESIAN_POINT('Ctrl Pts',(0.972506627935273,-0.00414265020170195,
2.57748752117621));
#21376=CARTESIAN_POINT('Ctrl Pts',(0.972521597304209,-0.00654688441944551,
2.57745933671442));
#21377=CARTESIAN_POINT('Ctrl Pts',(0.972586968658232,-0.0128156465435284,
2.57733627628346));
#21378=CARTESIAN_POINT('Ctrl Pts',(0.972653363288269,-0.016678636176991,
2.57721129835072));
#21379=CARTESIAN_POINT('Ctrl Pts',(0.972929256482295,-0.0281987946478753,
2.57669227394828));
#21380=CARTESIAN_POINT('Ctrl Pts',(0.973215079278776,-0.0358422720486581,
2.57615478699383));
#21381=CARTESIAN_POINT('Ctrl Pts',(0.974562717145952,-0.0623401377173552,
2.57362665221117));
#21382=CARTESIAN_POINT('Ctrl Pts',(0.976141626745025,-0.0810078079633483,
2.57067014303824));
#21383=CARTESIAN_POINT('Ctrl Pts',(0.980686505593143,-0.119336271682647,
2.56227318576719));
#21384=CARTESIAN_POINT('Ctrl Pts',(0.98374047439577,-0.138835225480723,
2.55667793110024));
#21385=CARTESIAN_POINT('Ctrl Pts',(0.987458837468451,-0.157876674355193,
2.55));
#21386=CARTESIAN_POINT('Ctrl Pts',(0.987454582400007,-0.157881308716372,
2.55005328965836));
#21387=CARTESIAN_POINT('Ctrl Pts',(0.987200786017512,-0.159467384180762,
2.5487918471679));
#21388=CARTESIAN_POINT('Ctrl Pts',(0.985506430965119,-0.169895526191808,
2.54029497054242));
#21389=CARTESIAN_POINT('Ctrl Pts',(0.982365078241419,-0.187417224408925,
2.52354132496555));
#21390=CARTESIAN_POINT('Ctrl Pts',(0.977999994055034,-0.208938409888944,
2.49656599568729));
#21391=CARTESIAN_POINT('Ctrl Pts',(0.971848592631414,-0.236216524025834,
2.45101723423612));
#21392=CARTESIAN_POINT('Ctrl Pts',(0.967372392238064,-0.253367892292085,
2.39214155711082));
#21393=CARTESIAN_POINT('Ctrl Pts',(0.967038345237899,-0.254607790735269,
2.32400532558939));
#21394=CARTESIAN_POINT('Ctrl Pts',(0.97062172581105,-0.241091125419321,
2.25963518301816));
#21395=CARTESIAN_POINT('Ctrl Pts',(0.978767296657426,-0.20640426202618,
2.19598850651528));
#21396=CARTESIAN_POINT('Ctrl Pts',(0.987595534630939,-0.160108842507484,
2.14787016428115));
#21397=CARTESIAN_POINT('Ctrl Pts',(0.995084474394307,-0.104856939129847,
2.11471063719305));
#21398=CARTESIAN_POINT('Ctrl Pts',(0.997930949375477,-0.066177461549665,
2.10319104189167));
#21399=CARTESIAN_POINT('Ctrl Pts',(0.998734041791771,-0.0502864579926989,
2.09999724006344));
#21400=CARTESIAN_POINT('Origin',(0.,0.,2.325));
#21401=CARTESIAN_POINT('',(-1.,-1.22464679914735E-16,2.55));
#21402=CARTESIAN_POINT('Origin',(0.,0.,2.55));
#21403=CARTESIAN_POINT('',(-0.157876674357314,0.987458837468112,2.54999999999916));
#21404=CARTESIAN_POINT('Origin',(0.,0.,2.55));
#21405=CARTESIAN_POINT('',(-0.0502392594122347,0.998737211088938,2.10000000017302));
#21406=CARTESIAN_POINT('Ctrl Pts',(-0.0501579437468834,0.998754980083996,
2.09996629680899));
#21407=CARTESIAN_POINT('Ctrl Pts',(-0.0826028085300709,0.997060472227549,
2.10669206239688));
#21408=CARTESIAN_POINT('Ctrl Pts',(-0.13333014615059,0.991871170579173,
2.12768221339602));
#21409=CARTESIAN_POINT('Ctrl Pts',(-0.184987608046235,0.98297944306662,
2.17252130019332));
#21410=CARTESIAN_POINT('Ctrl Pts',(-0.230530876255093,0.973454395083889,
2.2311541204646));
#21411=CARTESIAN_POINT('Ctrl Pts',(-0.255122284839583,0.966868905933786,
2.30756601931672));
#21412=CARTESIAN_POINT('Ctrl Pts',(-0.253875658998481,0.967246420818866,
2.38036927332879));
#21413=CARTESIAN_POINT('Ctrl Pts',(-0.237007380156922,0.971620587810882,
2.45580858562862));
#21414=CARTESIAN_POINT('Ctrl Pts',(-0.204967295321157,0.979117858283225,
2.50518732075992));
#21415=CARTESIAN_POINT('Ctrl Pts',(-0.173082478875929,0.984944804714717,
2.53735038518041));
#21416=CARTESIAN_POINT('Ctrl Pts',(-0.165770169783921,0.986201917446944,
2.54386940226406));
#21417=CARTESIAN_POINT('Ctrl Pts',(-0.157987843541269,0.987440871532657,
2.55001521460453));
#21418=CARTESIAN_POINT('Origin',(0.,0.,2.1));
#21419=CARTESIAN_POINT('Origin',(0.,0.,2.325));
#21420=CARTESIAN_POINT('',(0.0502392594122347,0.998737211088938,2.10000000017302));
#21421=CARTESIAN_POINT('Origin',(0.,0.,2.1));
#21422=CARTESIAN_POINT('',(0.157876674357314,0.987458837468112,2.54999999999916));
#21423=CARTESIAN_POINT('Ctrl Pts',(0.15787361447241,0.987459601094589,2.55002190145526));
#21424=CARTESIAN_POINT('Ctrl Pts',(0.159367603381274,0.987220783300611,
2.54883298459783));
#21425=CARTESIAN_POINT('Ctrl Pts',(0.16716148070395,0.985957317693993,2.54248953138653));
#21426=CARTESIAN_POINT('Ctrl Pts',(0.197782154055467,0.980628932028831,
2.51447081618292));
#21427=CARTESIAN_POINT('Ctrl Pts',(0.240862072091396,0.970821978192215,
2.45070211099161));
#21428=CARTESIAN_POINT('Ctrl Pts',(0.253753920072381,0.967257584978194,
2.38208598978509));
#21429=CARTESIAN_POINT('Ctrl Pts',(0.25377137321269,0.967257227319747,2.31770963275004));
#21430=CARTESIAN_POINT('Ctrl Pts',(0.247407872853293,0.96898626609141,2.28335835196792));
#21431=CARTESIAN_POINT('Ctrl Pts',(0.223542473616943,0.974765351154506,
2.22546113156583));
#21432=CARTESIAN_POINT('Ctrl Pts',(0.202625228604316,0.979486896662666,
2.19281789751093));
#21433=CARTESIAN_POINT('Ctrl Pts',(0.152664347670934,0.988739671565028,
2.14180432402534));
#21434=CARTESIAN_POINT('Ctrl Pts',(0.102949265500905,0.995581814195147,
2.11270476782457));
#21435=CARTESIAN_POINT('Ctrl Pts',(0.0581205001812461,0.998362457461274,
2.10152203482183));
#21436=CARTESIAN_POINT('Ctrl Pts',(0.0502611231985831,0.998755291180234,
2.09995263652274));
#21437=CARTESIAN_POINT('Origin',(0.,0.,2.55));
#21438=CARTESIAN_POINT('Origin',(0.705,0.,2.35));
#21439=CARTESIAN_POINT('',(0.501,-1.25526296912604E-17,2.145));
#21440=CARTESIAN_POINT('',(0.705,-2.51052593825207E-17,2.145));
#21441=CARTESIAN_POINT('',(0.457138928554548,-0.205,2.35));
#21442=CARTESIAN_POINT('Ctrl Pts',(0.457138928554548,-0.205,2.35));
#21443=CARTESIAN_POINT('Ctrl Pts',(0.457138928554548,-0.205,2.32390927987453));
#21444=CARTESIAN_POINT('Ctrl Pts',(0.459609069157102,-0.199722778787908,
2.29632432035936));
#21445=CARTESIAN_POINT('Ctrl Pts',(0.468177727272261,-0.178715671123715,
2.24592797085052));
#21446=CARTESIAN_POINT('Ctrl Pts',(0.474117890962221,-0.162998335554875,
2.22308455526839));
#21447=CARTESIAN_POINT('Ctrl Pts',(0.485018345626291,-0.126935588134045,
2.18702180784756));
#21448=CARTESIAN_POINT('Ctrl Pts',(0.490733376060334,-0.104084611878653,
2.17128923329376));
#21449=CARTESIAN_POINT('Ctrl Pts',(0.498772107838147,-0.0536585253249439,
2.1502704112139));
#21450=CARTESIAN_POINT('Ctrl Pts',(0.501,-0.0260615896504235,2.145));
#21451=CARTESIAN_POINT('Ctrl Pts',(0.501,-6.24500451351651E-17,2.145));
#21452=CARTESIAN_POINT('Ctrl Pts',(0.501,0.,2.145));
#21453=CARTESIAN_POINT('Ctrl Pts',(0.501,0.0260615896504235,2.145));
#21454=CARTESIAN_POINT('Ctrl Pts',(0.498772107838147,0.0536585253249438,
2.1502704112139));
#21455=CARTESIAN_POINT('Ctrl Pts',(0.490733376060334,0.104084611878653,
2.17128923329376));
#21456=CARTESIAN_POINT('Ctrl Pts',(0.485018345626291,0.126935588134045,
2.18702180784756));
#21457=CARTESIAN_POINT('Ctrl Pts',(0.474117890962221,0.162998335554875,
2.22308455526839));
#21458=CARTESIAN_POINT('Ctrl Pts',(0.468177727272261,0.178715671123715,
2.24592797085052));
#21459=CARTESIAN_POINT('Ctrl Pts',(0.459609069157102,0.199722778787908,
2.29632432035936));
#21460=CARTESIAN_POINT('Ctrl Pts',(0.457138928554548,0.205,2.32390927987453));
#21461=CARTESIAN_POINT('Ctrl Pts',(0.457138928554548,0.205,2.37609072012547));
#21462=CARTESIAN_POINT('Ctrl Pts',(0.459609069157102,0.199722778787908,
2.40367567964064));
#21463=CARTESIAN_POINT('Ctrl Pts',(0.468177727272261,0.178715671123715,
2.45407202914948));
#21464=CARTESIAN_POINT('Ctrl Pts',(0.474117890962221,0.162998335554875,
2.47691544473161));
#21465=CARTESIAN_POINT('Ctrl Pts',(0.485018345626291,0.126935588134045,
2.51297819215244));
#21466=CARTESIAN_POINT('Ctrl Pts',(0.490733376060334,0.104084611878653,
2.52871076670624));
#21467=CARTESIAN_POINT('Ctrl Pts',(0.498772107838147,0.0536585253249439,
2.5497295887861));
#21468=CARTESIAN_POINT('Ctrl Pts',(0.501,0.0260615896504235,2.555));
#21469=CARTESIAN_POINT('Ctrl Pts',(0.501,-0.0260615896504234,2.555));
#21470=CARTESIAN_POINT('Ctrl Pts',(0.498772107838147,-0.0536585253249438,
2.5497295887861));
#21471=CARTESIAN_POINT('Ctrl Pts',(0.490733376060334,-0.104084611878653,
2.52871076670624));
#21472=CARTESIAN_POINT('Ctrl Pts',(0.485018345626291,-0.126935588134045,
2.51297819215244));
#21473=CARTESIAN_POINT('Ctrl Pts',(0.474117890962222,-0.162998335554875,
2.47691544473161));
#21474=CARTESIAN_POINT('Ctrl Pts',(0.468177727272261,-0.178715671123715,
2.45407202914948));
#21475=CARTESIAN_POINT('Ctrl Pts',(0.459609069157102,-0.199722778787908,
2.40367567964064));
#21476=CARTESIAN_POINT('Ctrl Pts',(0.457138928554548,-0.205,2.37609072012547));
#21477=CARTESIAN_POINT('Ctrl Pts',(0.457138928554548,-0.205,2.35));
#21478=CARTESIAN_POINT('Ctrl Pts',(1.8740610339731E-6,0.999999999998244,
2.60499999999311));
#21479=CARTESIAN_POINT('Ctrl Pts',(-0.0335556196380034,1.00000006288704,
2.60500024661583));
#21480=CARTESIAN_POINT('Ctrl Pts',(-0.100756673071006,0.996441174833638,
2.59168345968582));
#21481=CARTESIAN_POINT('Ctrl Pts',(-0.157603488695687,0.98777358833807,
2.55296445525625));
#21482=CARTESIAN_POINT('Ctrl Pts',(-0.204967295321157,0.979117858283225,
2.50518732075992));
#21483=CARTESIAN_POINT('Ctrl Pts',(-0.237007380156922,0.971620587810882,
2.45580858562862));
#21484=CARTESIAN_POINT('Ctrl Pts',(-0.253875658998481,0.967246420818866,
2.38036927332879));
#21485=CARTESIAN_POINT('Ctrl Pts',(-0.255122284839583,0.966868905933786,
2.30756601931672));
#21486=CARTESIAN_POINT('Ctrl Pts',(-0.230530876255093,0.973454395083889,
2.2311541204646));
#21487=CARTESIAN_POINT('Ctrl Pts',(-0.184987608046235,0.98297944306662,
2.17252130019332));
#21488=CARTESIAN_POINT('Ctrl Pts',(-0.130000247114384,0.992444341497521,
2.12479183461179));
#21489=CARTESIAN_POINT('Ctrl Pts',(-0.0547900546441262,0.999800917250482,
2.09586490599377));
#21490=CARTESIAN_POINT('Ctrl Pts',(0.00901292386013043,1.00025490450459,
2.09401178448709));
#21491=CARTESIAN_POINT('Ctrl Pts',(0.0460479466138129,0.999088187246804,
2.09861314679373));
#21492=CARTESIAN_POINT('Ctrl Pts',(0.101662133244068,0.995758958476132,
2.11195137517568));
#21493=CARTESIAN_POINT('Ctrl Pts',(0.152664347670934,0.988739671565028,
2.14180432402534));
#21494=CARTESIAN_POINT('Ctrl Pts',(0.202625228604316,0.979486896662666,
2.19281789751093));
#21495=CARTESIAN_POINT('Ctrl Pts',(0.223542473616943,0.974765351154506,
2.22546113156583));
#21496=CARTESIAN_POINT('Ctrl Pts',(0.247407872853293,0.96898626609141,2.28335835196792));
#21497=CARTESIAN_POINT('Ctrl Pts',(0.25377137321269,0.967257227319747,2.31770963275004));
#21498=CARTESIAN_POINT('Ctrl Pts',(0.253753920072381,0.967257584978194,
2.38208598978509));
#21499=CARTESIAN_POINT('Ctrl Pts',(0.240862072091396,0.970821978192215,
2.45070211099161));
#21500=CARTESIAN_POINT('Ctrl Pts',(0.197782154055467,0.980628932028831,
2.51447081618292));
#21501=CARTESIAN_POINT('Ctrl Pts',(0.16267570908935,0.986737898868484,2.54659412947604));
#21502=CARTESIAN_POINT('Ctrl Pts',(0.136234199434897,0.990851168416345,
2.56664374352278));
#21503=CARTESIAN_POINT('Ctrl Pts',(0.0840473157184407,0.997329420352096,
2.59494454511583));
#21504=CARTESIAN_POINT('Ctrl Pts',(0.03365753814838,0.999999936925475,2.60499975264892));
#21505=CARTESIAN_POINT('Ctrl Pts',(1.8740610339731E-6,0.999999999998244,
2.60499999999311));
#21506=CARTESIAN_POINT('Ctrl Pts',(1.72646341657069E-6,0.983333333331803,
2.58833333332708));
#21507=CARTESIAN_POINT('Ctrl Pts',(-0.0309211194933883,0.983327802047045,
2.58831966882739));
#21508=CARTESIAN_POINT('Ctrl Pts',(-0.0928377960476621,0.98023976768212,
2.57629404074584));
#21509=CARTESIAN_POINT('Ctrl Pts',(-0.146048423576797,0.972626976944164,
2.54070953195264));
#21510=CARTESIAN_POINT('Ctrl Pts',(-0.190747496194426,0.964977664234015,
2.49636747507197));
#21511=CARTESIAN_POINT('Ctrl Pts',(-0.221374849129247,0.95831490086092,
2.45011538765543));
#21512=CARTESIAN_POINT('Ctrl Pts',(-0.237650481571607,0.954402200933291,
2.37878285196974));
#21513=CARTESIAN_POINT('Ctrl Pts',(-0.238858199349336,0.954071300725052,
2.30977107620483));
#21514=CARTESIAN_POINT('Ctrl Pts',(-0.215099921034606,0.959955138122488,
2.23759648199501));
#21515=CARTESIAN_POINT('Ctrl Pts',(-0.17183883952112,0.968399947196108,
2.18290355895676));
#21516=CARTESIAN_POINT('Ctrl Pts',(-0.120099054224975,0.976743248230922,
2.13876052168788));
#21517=CARTESIAN_POINT('Ctrl Pts',(-0.0504163434655785,0.983158893045571,
2.11245900795287));
#21518=CARTESIAN_POINT('Ctrl Pts',(0.00827833993718029,0.983561344274991,
2.1107555539468));
#21519=CARTESIAN_POINT('Ctrl Pts',(0.0424518621317906,0.982538668939213,
2.11495120932668));
#21520=CARTESIAN_POINT('Ctrl Pts',(0.0937720299455498,0.979640570051344,
2.12707976132422));
#21521=CARTESIAN_POINT('Ctrl Pts',(0.141360481904814,0.973477223378796,
2.15443787690997));
#21522=CARTESIAN_POINT('Ctrl Pts',(0.188538345234594,0.965310317630362,
2.20179163355866));
#21523=CARTESIAN_POINT('Ctrl Pts',(0.208490757001602,0.961105657569896,
2.23236164151278));
#21524=CARTESIAN_POINT('Ctrl Pts',(0.231400254955185,0.955964354544338,
2.28688145033855));
#21525=CARTESIAN_POINT('Ctrl Pts',(0.237544330067899,0.954413219989739,
2.31941255684048));
#21526=CARTESIAN_POINT('Ctrl Pts',(0.237537755869605,0.954418441564086,
2.38038851320367));
#21527=CARTESIAN_POINT('Ctrl Pts',(0.225032695661137,0.957606932779055,
2.44537253850971));
#21528=CARTESIAN_POINT('Ctrl Pts',(0.183910350012796,0.966318757498156,
2.50501316984723));
#21529=CARTESIAN_POINT('Ctrl Pts',(0.150857782836235,0.971711641804196,
2.53478061849988));
#21530=CARTESIAN_POINT('Ctrl Pts',(0.126062259734711,0.975331110231934,
2.55328561568025));
#21531=CARTESIAN_POINT('Ctrl Pts',(0.0774389729843563,0.981016367853088,
2.57924416260037));
#21532=CARTESIAN_POINT('Ctrl Pts',(0.0310095625324942,0.983324489370319,
2.58831441049439));
#21533=CARTESIAN_POINT('Ctrl Pts',(1.72646341657069E-6,0.983333333331803,
2.58833333332708));
#21534=CARTESIAN_POINT('Ctrl Pts',(1.57886579916828E-6,0.966666666665363,
2.57166666666104));
#21535=CARTESIAN_POINT('Ctrl Pts',(-0.028261782201734,0.966672299451083,
2.57168075671789));
#21536=CARTESIAN_POINT('Ctrl Pts',(-0.0849369725180309,0.964038061600584,
2.56088137505698));
#21537=CARTESIAN_POINT('Ctrl Pts',(-0.134467081311291,0.957489301980934,
2.52849464185));
#21538=CARTESIAN_POINT('Ctrl Pts',(-0.176493077367449,0.950850885491106,
2.48751717131812));
#21539=CARTESIAN_POINT('Ctrl Pts',(-0.205749279945383,0.945011607194673,
2.44443170330968));
#21540=CARTESIAN_POINT('Ctrl Pts',(-0.221405615759076,0.941576404880082,
2.37718285612148));
#21541=CARTESIAN_POINT('Ctrl Pts',(-0.222592256095046,0.941273043800734,
2.31198020634687));
#21542=CARTESIAN_POINT('Ctrl Pts',(-0.19967059846768,0.946452066132863,
2.24404982314633));
#21543=CARTESIAN_POINT('Ctrl Pts',(-0.158679713896286,0.953815819341673,
2.19329233666131));
#21544=CARTESIAN_POINT('Ctrl Pts',(-0.110198993644362,0.961036297799555,
2.15273846356872));
#21545=CARTESIAN_POINT('Ctrl Pts',(-0.046075343884759,0.966525769606431,
2.12903238312702));
#21546=CARTESIAN_POINT('Ctrl Pts',(0.00757919676247354,0.966850980745995,
2.12753983018364));
#21547=CARTESIAN_POINT('Ctrl Pts',(0.0388114474174279,0.965990205488828,
2.13128917659776));
#21548=CARTESIAN_POINT('Ctrl Pts',(0.0859427838572395,0.963505820548163,
2.14224095850635));
#21549=CARTESIAN_POINT('Ctrl Pts',(0.130095057847622,0.958228990545236,
2.16703937038342));
#21550=CARTESIAN_POINT('Ctrl Pts',(0.17448083867517,0.95111834103327,2.21079555546396));
#21551=CARTESIAN_POINT('Ctrl Pts',(0.193473476747956,0.947464227672504,
2.23924962741081));
#21552=CARTESIAN_POINT('Ctrl Pts',(0.215362766008526,0.942940862740997,
2.29040473546289));
#21553=CARTESIAN_POINT('Ctrl Pts',(0.221328116324425,0.941582271034106,
2.32111335094323));
#21554=CARTESIAN_POINT('Ctrl Pts',(0.221307475198179,0.941576462552143,
2.37869131092512));
#21555=CARTESIAN_POINT('Ctrl Pts',(0.209212867982546,0.944395419867102,
2.44004063866257));
#21556=CARTESIAN_POINT('Ctrl Pts',(0.170035598298793,0.952016482602868,
2.49557168347949));
#21557=CARTESIAN_POINT('Ctrl Pts',(0.139037988014577,0.956682144907831,
2.52295666497662));
#21558=CARTESIAN_POINT('Ctrl Pts',(0.115891644338605,0.959813980610051,
2.53993061096407));
#21559=CARTESIAN_POINT('Ctrl Pts',(0.0708540967431303,0.964686661475804,
2.56350215110508));
#21560=CARTESIAN_POINT('Ctrl Pts',(0.0283530954373026,0.96667540882895,
2.57168516269162));
#21561=CARTESIAN_POINT('Ctrl Pts',(1.57886579916828E-6,0.966666666665363,
2.57166666666104));
#21562=CARTESIAN_POINT('Ctrl Pts',(1.43126818176587E-6,0.949999999998922,
2.554999999995));
#21563=CARTESIAN_POINT('Ctrl Pts',(-0.0256272820571188,0.950000038611092,
2.55500017892945));
#21564=CARTESIAN_POINT('Ctrl Pts',(-0.0770180954946874,0.947836654449066,
2.545491956117));
#21565=CARTESIAN_POINT('Ctrl Pts',(-0.122912016192401,0.942342690587028,
2.51623971854639));
#21566=CARTESIAN_POINT('Ctrl Pts',(-0.162273278240718,0.936710691441896,
2.47869732563017));
#21567=CARTESIAN_POINT('Ctrl Pts',(-0.190116748917708,0.931705920244711,
2.43873850533649));
#21568=CARTESIAN_POINT('Ctrl Pts',(-0.205180438332203,0.928732184994508,
2.37559643476243));
#21569=CARTESIAN_POINT('Ctrl Pts',(-0.2063281706048,0.928475438592001,2.31418526323498));
#21570=CARTESIAN_POINT('Ctrl Pts',(-0.184239643247193,0.932952809171462,
2.25049218467674));
#21571=CARTESIAN_POINT('Ctrl Pts',(-0.14553094537117,0.939236323471161,
2.20367459542476));
#21572=CARTESIAN_POINT('Ctrl Pts',(-0.100297800754953,0.945335204532955,
2.16670715064481));
#21573=CARTESIAN_POINT('Ctrl Pts',(-0.0417016327062113,0.94988374540152,
2.14562648508612));
#21574=CARTESIAN_POINT('Ctrl Pts',(0.0068446128395234,0.950157420516395,
2.14428359964335));
#21575=CARTESIAN_POINT('Ctrl Pts',(0.0352153629354055,0.949440687181237,
2.14762723913071));
#21576=CARTESIAN_POINT('Ctrl Pts',(0.0780526805587212,0.947387432123376,
2.15736934465489));
#21577=CARTESIAN_POINT('Ctrl Pts',(0.118791192081503,0.942966542359005,
2.17967292326805));
#21578=CARTESIAN_POINT('Ctrl Pts',(0.160393955305448,0.936941762000965,
2.2197692915117));
#21579=CARTESIAN_POINT('Ctrl Pts',(0.178421760132616,0.933804534087895,
2.24615013735776));
#21580=CARTESIAN_POINT('Ctrl Pts',(0.199355148110418,0.929918951193924,
2.29392783383353));
#21581=CARTESIAN_POINT('Ctrl Pts',(0.205101073179634,0.928738263704097,
2.32281627503367));
#21582=CARTESIAN_POINT('Ctrl Pts',(0.205091310995403,0.928737319138035,
2.3769938343437));
#21583=CARTESIAN_POINT('Ctrl Pts',(0.193383491552286,0.931180374453942,
2.43471106618067));
#21584=CARTESIAN_POINT('Ctrl Pts',(0.156163794256122,0.937706308072193,
2.4861140371438));
#21585=CARTESIAN_POINT('Ctrl Pts',(0.127220061761462,0.941655887843543,
2.51114315400046));
#21586=CARTESIAN_POINT('Ctrl Pts',(0.105719704638418,0.944293922425639,
2.52657248312153));
#21587=CARTESIAN_POINT('Ctrl Pts',(0.0642457540090459,0.948373608976796,
2.54780176858962));
#21588=CARTESIAN_POINT('Ctrl Pts',(0.0257051198214169,0.949999961273794,
2.55499982053709));
#21589=CARTESIAN_POINT('Ctrl Pts',(1.43126818176587E-6,0.949999999998922,
2.554999999995));
#21590=CARTESIAN_POINT('Ctrl Pts',(-0.0501579420662037,0.998754980171774,
2.09996629646059));
#21591=CARTESIAN_POINT('Ctrl Pts',(-0.0455541516249309,0.998081971740583,
2.09994285225375));
#21592=CARTESIAN_POINT('Ctrl Pts',(-0.0409493960495382,0.997497248478843,
2.09992115702739));
#21593=CARTESIAN_POINT('Ctrl Pts',(-0.0363408599228962,0.997001962981805,
2.0999069394429));
#21594=CARTESIAN_POINT('Ctrl Pts',(-0.0344254769968775,0.996796114235378,
2.09990103038244));
#21595=CARTESIAN_POINT('Ctrl Pts',(-0.0325094393882293,0.996605701141417,
2.09989644467646));
#21596=CARTESIAN_POINT('Ctrl Pts',(-0.030591027199469,0.996431064903213,
2.0998929904383));
#21597=CARTESIAN_POINT('Ctrl Pts',(-0.0241570348712139,0.995845367927649,
2.09988140557563));
#21598=CARTESIAN_POINT('Ctrl Pts',(-0.0177195435991528,0.995439341015549,
2.09988208911745));
#21599=CARTESIAN_POINT('Ctrl Pts',(-0.0112042061332443,0.99522006377236,
2.09989207709953));
#21600=CARTESIAN_POINT('Ctrl Pts',(-0.0091395956891891,0.995150578179511,
2.09989524213775));
#21601=CARTESIAN_POINT('Ctrl Pts',(-0.00706875291999245,0.995099879623312,
2.09989939288935));
#21602=CARTESIAN_POINT('Ctrl Pts',(-0.00498909077113959,0.995068038205673,
2.09990458544879));
#21603=CARTESIAN_POINT('Ctrl Pts',(-0.00372411379059672,0.995048670319229,
2.09990774387919));
#21604=CARTESIAN_POINT('Ctrl Pts',(-0.00245612535390708,0.995036282497343,
2.09991128863539));
#21605=CARTESIAN_POINT('Ctrl Pts',(-0.00118453247084987,0.995030876493846,
2.09991524595687));
#21606=CARTESIAN_POINT('Ctrl Pts',(-4.37845315938809E-5,0.995026026759759,
2.09991879607608));
#21607=CARTESIAN_POINT('Ctrl Pts',(0.00109970303547405,0.995026788370882,
2.09992271042795));
#21608=CARTESIAN_POINT('Ctrl Pts',(0.00223928716687367,0.995033203141033,
2.09992682811702));
#21609=CARTESIAN_POINT('Ctrl Pts',(0.0036616886009847,0.995041209902455,
2.09993196771721));
#21610=CARTESIAN_POINT('Ctrl Pts',(0.00508052255109117,0.995058026539435,
2.09993740601942));
#21611=CARTESIAN_POINT('Ctrl Pts',(0.00649660255618722,0.99508373088496,
2.09994278957186));
#21612=CARTESIAN_POINT('Ctrl Pts',(0.00927146453168093,0.99513409951579,
2.09995333884513));
#21613=CARTESIAN_POINT('Ctrl Pts',(0.0120342525028786,0.995218575771198,
2.09996364717532));
#21614=CARTESIAN_POINT('Ctrl Pts',(0.0147909036437984,0.995337528356299,
2.0999713663429));
#21615=CARTESIAN_POINT('Ctrl Pts',(0.0158423647792016,0.995382900082279,
2.09997431064172));
#21616=CARTESIAN_POINT('Ctrl Pts',(0.0168924947237524,0.995433267490783,
2.09997688114622));
#21617=CARTESIAN_POINT('Ctrl Pts',(0.0179416114429507,0.995488633595717,
2.09997896362948));
#21618=CARTESIAN_POINT('Ctrl Pts',(0.0227736532195703,0.995743639856846,
2.09998855517054));
#21619=CARTESIAN_POINT('Ctrl Pts',(0.027584328345019,0.996104743818564,
2.09998770209067));
#21620=CARTESIAN_POINT('Ctrl Pts',(0.0323893668042188,0.996568206430001,
2.09998210436156));
#21621=CARTESIAN_POINT('Ctrl Pts',(0.0368950513274315,0.997002795316889,
2.09997685537102));
#21622=CARTESIAN_POINT('Ctrl Pts',(0.0413861399780065,0.997526459114176,
2.09996745668706));
#21623=CARTESIAN_POINT('Ctrl Pts',(0.0458741854723339,0.99813430097851,
2.09995967180744));
#21624=CARTESIAN_POINT('Ctrl Pts',(0.0473368418337277,0.998332396958311,
2.09995713471112));
#21625=CARTESIAN_POINT('Ctrl Pts',(0.0487991635875438,0.99853942952464,
2.09995477525694));
#21626=CARTESIAN_POINT('Ctrl Pts',(0.0502611215119263,0.998755291264538,
2.09995263618594));
#21627=CARTESIAN_POINT('',(1.63052496528509E-6,0.972500000001548,2.57749999999709));
#21628=CARTESIAN_POINT('Ctrl Pts',(-0.157876674355192,0.987458837468451,
2.55));
#21629=CARTESIAN_POINT('Ctrl Pts',(-0.14679428096426,0.985294697406766,
2.55388665064189));
#21630=CARTESIAN_POINT('Ctrl Pts',(-0.135549889588828,0.983354421647031,
2.55740912752908));
#21631=CARTESIAN_POINT('Ctrl Pts',(-0.0935709003424397,0.977055328631449,
2.56892572544489));
#21632=CARTESIAN_POINT('Ctrl Pts',(-0.062201374246487,0.974161715360584,
2.57437596695135));
#21633=CARTESIAN_POINT('Ctrl Pts',(-0.024619403298166,0.972834706545006,
2.57687004873351));
#21634=CARTESIAN_POINT('Ctrl Pts',(-0.0189840464089389,0.972691422895011,
2.57713968402705));
#21635=CARTESIAN_POINT('Ctrl Pts',(-0.0105124985263454,0.972559701868467,
2.57738760007473));
#21636=CARTESIAN_POINT('Ctrl Pts',(-0.00768142954473445,0.972529696233088,
2.5774440907214));
#21637=CARTESIAN_POINT('Ctrl Pts',(-0.0032326711402507,0.972504563213093,
2.57749140831944));
#21638=CARTESIAN_POINT('Ctrl Pts',(-0.0016155351650678,0.972499996930093,
2.57750000577993));
#21639=CARTESIAN_POINT('Ctrl Pts',(1.63052496528509E-6,0.972500000001548,
2.57749999999708));
#21640=CARTESIAN_POINT('',(1.43126818176587E-6,0.949999999998922,2.554999999995));
#21641=CARTESIAN_POINT('Ctrl Pts',(1.63052496528509E-6,0.972500000001548,
2.57749999999709));
#21642=CARTESIAN_POINT('Ctrl Pts',(1.56410603744535E-6,0.965000000000673,
2.56999999999639));
#21643=CARTESIAN_POINT('Ctrl Pts',(1.49768710960561E-6,0.957499999999797,
2.5624999999957));
#21644=CARTESIAN_POINT('Ctrl Pts',(1.43126818176587E-6,0.949999999998922,
2.554999999995));
#21645=CARTESIAN_POINT('',(-3.4869210388678E-5,0.950019014087066,2.14494180214374));
#21646=CARTESIAN_POINT('Ctrl Pts',(1.43126818176587E-6,0.949999999998922,
2.554999999995));
#21647=CARTESIAN_POINT('Ctrl Pts',(-0.0256272820571188,0.950000038611092,
2.55500017892945));
#21648=CARTESIAN_POINT('Ctrl Pts',(-0.0770180954946874,0.947836654449066,
2.545491956117));
#21649=CARTESIAN_POINT('Ctrl Pts',(-0.122912016192401,0.942342690587028,
2.51623971854639));
#21650=CARTESIAN_POINT('Ctrl Pts',(-0.162273278240718,0.936710691441896,
2.47869732563017));
#21651=CARTESIAN_POINT('Ctrl Pts',(-0.190116748917708,0.931705920244711,
2.43873850533649));
#21652=CARTESIAN_POINT('Ctrl Pts',(-0.205180438332203,0.928732184994508,
2.37559643476243));
#21653=CARTESIAN_POINT('Ctrl Pts',(-0.2063281706048,0.928475438592001,2.31418526323498));
#21654=CARTESIAN_POINT('Ctrl Pts',(-0.184239643247193,0.932952809171462,
2.25049218467674));
#21655=CARTESIAN_POINT('Ctrl Pts',(-0.14553094537117,0.939236323471161,
2.20367459542476));
#21656=CARTESIAN_POINT('Ctrl Pts',(-0.100297800754953,0.945335204532955,
2.16670715064481));
#21657=CARTESIAN_POINT('Ctrl Pts',(-0.0465835707283805,0.949504783852479,
2.14738282011878));
#21658=CARTESIAN_POINT('Ctrl Pts',(-0.00936425895417839,0.950027004161095,
2.14491207293051));
#21659=CARTESIAN_POINT('Ctrl Pts',(-3.48692103886768E-5,0.950019014087066,
2.14494180214374));
#21660=CARTESIAN_POINT('Ctrl Pts',(-3.48692103886768E-5,0.950019014087066,
2.14494180214374));
#21661=CARTESIAN_POINT('Ctrl Pts',(0.00462828401910463,0.950015020370377,
2.14495666183772));
#21662=CARTESIAN_POINT('Ctrl Pts',(0.0163025714633961,0.949918483082405,
2.14539826893541));
#21663=CARTESIAN_POINT('Ctrl Pts',(0.0352153629354055,0.949440687181237,
2.14762723913071));
#21664=CARTESIAN_POINT('Ctrl Pts',(0.0780526805587212,0.947387432123376,
2.15736934465489));
#21665=CARTESIAN_POINT('Ctrl Pts',(0.118791192081503,0.942966542359005,
2.17967292326805));
#21666=CARTESIAN_POINT('Ctrl Pts',(0.160393955305448,0.936941762000965,
2.2197692915117));
#21667=CARTESIAN_POINT('Ctrl Pts',(0.178421760132616,0.933804534087895,
2.24615013735776));
#21668=CARTESIAN_POINT('Ctrl Pts',(0.199355148110418,0.929918951193924,
2.29392783383353));
#21669=CARTESIAN_POINT('Ctrl Pts',(0.205101073179634,0.928738263704097,
2.32281627503367));
#21670=CARTESIAN_POINT('Ctrl Pts',(0.205091310995403,0.928737319138035,
2.3769938343437));
#21671=CARTESIAN_POINT('Ctrl Pts',(0.193383491552286,0.931180374453942,
2.43471106618067));
#21672=CARTESIAN_POINT('Ctrl Pts',(0.156163794256122,0.937706308072193,
2.4861140371438));
#21673=CARTESIAN_POINT('Ctrl Pts',(0.127220061761462,0.941655887843543,
2.51114315400046));
#21674=CARTESIAN_POINT('Ctrl Pts',(0.105719704638418,0.944293922425639,
2.52657248312153));
#21675=CARTESIAN_POINT('Ctrl Pts',(0.0642457540090459,0.948373608976796,
2.54780176858962));
#21676=CARTESIAN_POINT('Ctrl Pts',(0.0257051198214169,0.949999961273794,
2.55499982053709));
#21677=CARTESIAN_POINT('Ctrl Pts',(1.43126818176587E-6,0.949999999998922,
2.554999999995));
#21678=CARTESIAN_POINT('Ctrl Pts',(1.63052496528509E-6,0.972500000001548,
2.57749999999708));
#21679=CARTESIAN_POINT('Ctrl Pts',(0.000580473862567526,0.972500001100936,
2.57749999792719));
#21680=CARTESIAN_POINT('Ctrl Pts',(0.00115932100720228,0.972500587629742,
2.5774988936244));
#21681=CARTESIAN_POINT('Ctrl Pts',(0.00414265020169645,0.972506627935274,
2.57748752117621));
#21682=CARTESIAN_POINT('Ctrl Pts',(0.00654688441943462,0.972521597304209,
2.57745933671442));
#21683=CARTESIAN_POINT('Ctrl Pts',(0.0128156465435042,0.972586968658231,
2.57733627628346));
#21684=CARTESIAN_POINT('Ctrl Pts',(0.0166786361769429,0.972653363288268,
2.57721129835072));
#21685=CARTESIAN_POINT('Ctrl Pts',(0.0281987946478794,0.972929256482295,
2.57669227394828));
#21686=CARTESIAN_POINT('Ctrl Pts',(0.0358422720486675,0.973215079278776,
2.57615478699383));
#21687=CARTESIAN_POINT('Ctrl Pts',(0.0623401377173534,0.974562717145952,
2.57362665221117));
#21688=CARTESIAN_POINT('Ctrl Pts',(0.0810078079633459,0.976141626745025,
2.57067014303824));
#21689=CARTESIAN_POINT('Ctrl Pts',(0.119336271682641,0.980686505593142,
2.56227318576719));
#21690=CARTESIAN_POINT('Ctrl Pts',(0.138835225480719,0.983740474395769,
2.55667793110024));
#21691=CARTESIAN_POINT('Ctrl Pts',(0.157876674355193,0.987458837468451,
2.55));
#21692=CARTESIAN_POINT('Origin',(4.31687996699442E-17,0.705,2.35));
#21693=CARTESIAN_POINT('',(-0.205,0.457138928554548,2.35));
#21694=CARTESIAN_POINT('',(-1.45611632917078E-17,0.501,2.145));
#21695=CARTESIAN_POINT('Ctrl Pts',(-0.205,0.457138928554548,2.35));
#21696=CARTESIAN_POINT('Ctrl Pts',(-0.205,0.457138928554548,2.37609072012547));
#21697=CARTESIAN_POINT('Ctrl Pts',(-0.199722778787908,0.459609069157102,
2.40367567964064));
#21698=CARTESIAN_POINT('Ctrl Pts',(-0.178715671123715,0.468177727272261,
2.45407202914948));
#21699=CARTESIAN_POINT('Ctrl Pts',(-0.162998335554875,0.474117890962222,
2.47691544473161));
#21700=CARTESIAN_POINT('Ctrl Pts',(-0.126935588134045,0.485018345626291,
2.51297819215244));
#21701=CARTESIAN_POINT('Ctrl Pts',(-0.104084611878653,0.490733376060334,
2.52871076670624));
#21702=CARTESIAN_POINT('Ctrl Pts',(-0.0536585253249438,0.498772107838147,
2.5497295887861));
#21703=CARTESIAN_POINT('Ctrl Pts',(-0.0260615896504234,0.501,2.555));
#21704=CARTESIAN_POINT('Ctrl Pts',(0.0260615896504235,0.501,2.555));
#21705=CARTESIAN_POINT('Ctrl Pts',(0.0536585253249439,0.498772107838147,
2.5497295887861));
#21706=CARTESIAN_POINT('Ctrl Pts',(0.104084611878653,0.490733376060334,
2.52871076670624));
#21707=CARTESIAN_POINT('Ctrl Pts',(0.126935588134046,0.485018345626291,
2.51297819215244));
#21708=CARTESIAN_POINT('Ctrl Pts',(0.162998335554875,0.474117890962221,
2.47691544473161));
#21709=CARTESIAN_POINT('Ctrl Pts',(0.178715671123715,0.468177727272261,
2.45407202914948));
#21710=CARTESIAN_POINT('Ctrl Pts',(0.199722778787908,0.459609069157102,
2.40367567964064));
#21711=CARTESIAN_POINT('Ctrl Pts',(0.205,0.457138928554548,2.37609072012547));
#21712=CARTESIAN_POINT('Ctrl Pts',(0.205,0.457138928554548,2.32390927987453));
#21713=CARTESIAN_POINT('Ctrl Pts',(0.199722778787908,0.459609069157102,
2.29632432035936));
#21714=CARTESIAN_POINT('Ctrl Pts',(0.178715671123715,0.468177727272261,
2.24592797085052));
#21715=CARTESIAN_POINT('Ctrl Pts',(0.162998335554875,0.474117890962221,
2.22308455526839));
#21716=CARTESIAN_POINT('Ctrl Pts',(0.126935588134045,0.485018345626291,
2.18702180784756));
#21717=CARTESIAN_POINT('Ctrl Pts',(0.104084611878653,0.490733376060334,
2.17128923329376));
#21718=CARTESIAN_POINT('Ctrl Pts',(0.0536585253249439,0.498772107838147,
2.1502704112139));
#21719=CARTESIAN_POINT('Ctrl Pts',(0.0260615896504234,0.501,2.145));
#21720=CARTESIAN_POINT('Ctrl Pts',(-3.46944695195361E-17,0.501,2.145));
#21721=CARTESIAN_POINT('Ctrl Pts',(-3.46944695195361E-17,0.501,2.145));
#21722=CARTESIAN_POINT('Ctrl Pts',(-0.0260615896504235,0.501,2.145));
#21723=CARTESIAN_POINT('Ctrl Pts',(-0.0536585253249439,0.498772107838147,
2.1502704112139));
#21724=CARTESIAN_POINT('Ctrl Pts',(-0.104084611878653,0.490733376060334,
2.17128923329376));
#21725=CARTESIAN_POINT('Ctrl Pts',(-0.126935588134045,0.485018345626291,
2.18702180784756));
#21726=CARTESIAN_POINT('Ctrl Pts',(-0.162998335554875,0.474117890962221,
2.22308455526839));
#21727=CARTESIAN_POINT('Ctrl Pts',(-0.178715671123715,0.468177727272261,
2.24592797085052));
#21728=CARTESIAN_POINT('Ctrl Pts',(-0.199722778787908,0.459609069157102,
2.29632432035936));
#21729=CARTESIAN_POINT('Ctrl Pts',(-0.205,0.457138928554548,2.32390927987453));
#21730=CARTESIAN_POINT('Ctrl Pts',(-0.205,0.457138928554548,2.35));
#21731=CARTESIAN_POINT('',(1.80635402874235E-17,0.705,2.145));
#21732=CARTESIAN_POINT('Origin',(0.,0.,2.575));
#21733=CARTESIAN_POINT('',(-0.95,-1.16341445918999E-16,2.6));
#21734=CARTESIAN_POINT('Origin',(0.,0.,2.6));
#21735=CARTESIAN_POINT('',(-0.975,-1.19403062916867E-16,2.575));
#21736=CARTESIAN_POINT('Ctrl Pts',(0.958722904333223,-0.492368803403902,
1.28318567027397));
#21737=CARTESIAN_POINT('Ctrl Pts',(1.17966054547972,-0.551909716442828,
1.53751096017971));
#21738=CARTESIAN_POINT('Ctrl Pts',(1.38346957888851,-0.474301142999537,
1.74607168007007));
#21739=CARTESIAN_POINT('Ctrl Pts',(1.57015000455958,-0.25954308307403,1.90886782994505));
#21740=CARTESIAN_POINT('Ctrl Pts',(0.977056147031499,-0.499517476440598,
1.26357731004417));
#21741=CARTESIAN_POINT('Ctrl Pts',(1.20215092434677,-0.559685710444569,
1.51399891879435));
#21742=CARTESIAN_POINT('Ctrl Pts',(1.40943351079342,-0.480379041610332,
1.71946418982835));
#21743=CARTESIAN_POINT('Ctrl Pts',(1.59908490462109,-0.261294297877456,
1.87976839865854));
#21744=CARTESIAN_POINT('Ctrl Pts',(1.00746303394202,-0.518620069692388,
1.22814769645102));
#21745=CARTESIAN_POINT('Ctrl Pts',(1.23972845750293,-0.581473014736936,
1.47151503544581));
#21746=CARTESIAN_POINT('Ctrl Pts',(1.45412237507391,-0.500093997069209,
1.67108761359797));
#21747=CARTESIAN_POINT('Ctrl Pts',(1.65065338225238,-0.274488870722725,
1.82686083829874));
#21748=CARTESIAN_POINT('Ctrl Pts',(1.04993028655864,-0.572066424422519,
1.16792151434878));
#21749=CARTESIAN_POINT('Ctrl Pts',(1.2934389287759,-0.644190775510559,1.39927831144435));
#21750=CARTESIAN_POINT('Ctrl Pts',(1.52163836885008,-0.563757672145161,
1.58904291706244));
#21751=CARTESIAN_POINT('Ctrl Pts',(1.73461532684231,-0.33063289130358,1.73712011416644));
#21752=CARTESIAN_POINT('Ctrl Pts',(1.07500617197391,-0.618955132624418,
1.12620659350916));
#21753=CARTESIAN_POINT('Ctrl Pts',(1.32576077930413,-0.699668038277416,
1.34934531900258));
#21754=CARTESIAN_POINT('Ctrl Pts',(1.5644313526713,-0.621802268592357,1.53232296148774));
#21755=CARTESIAN_POINT('Ctrl Pts',(1.79095608809519,-0.385229355344034,
1.67514376227794));
#21756=CARTESIAN_POINT('Ctrl Pts',(1.08812946536139,-0.649605006049397,
1.10192284729582));
#21757=CARTESIAN_POINT('Ctrl Pts',(1.34295142581462,-0.736085457637468,
1.32027771712106));
#21758=CARTESIAN_POINT('Ctrl Pts',(1.58796351671871,-0.660325994321481,
1.4993370241196));
#21759=CARTESIAN_POINT('Ctrl Pts',(1.82316573807368,-0.422326616101437,
1.63910076829143));
#21760=CARTESIAN_POINT('',(0.962275025729455,-0.493314642657339,1.28727233489076));
#21761=CARTESIAN_POINT('',(1.08521613661244,-0.642908916934723,1.10727038327973));
#21762=CARTESIAN_POINT('Ctrl Pts',(0.962275025729455,-0.493314642657339,
1.28727233489076));
#21763=CARTESIAN_POINT('Ctrl Pts',(0.992714976574291,-0.505155444616777,
1.25478273943474));
#21764=CARTESIAN_POINT('Ctrl Pts',(1.01347020049701,-0.522900410113937,
1.22829923781273));
#21765=CARTESIAN_POINT('Ctrl Pts',(1.05095536138695,-0.572202237706898,
1.17205963503468));
#21766=CARTESIAN_POINT('Ctrl Pts',(1.0691927306699,-0.603178396559865,1.14130666672664));
#21767=CARTESIAN_POINT('Ctrl Pts',(1.08521613661244,-0.642908916934723,
1.10727038327973));
#21768=CARTESIAN_POINT('',(1.5699559447672,-0.259766273896474,1.90869858745619));
#21769=CARTESIAN_POINT('Ctrl Pts',(0.962275025729455,-0.493314642657339,
1.28727233489076));
#21770=CARTESIAN_POINT('Ctrl Pts',(1.06019965524839,-0.519074140629025,
1.39987124007464));
#21771=CARTESIAN_POINT('Ctrl Pts',(1.15475382712427,-0.517846241724568,
1.50346488650363));
#21772=CARTESIAN_POINT('Ctrl Pts',(1.35913828497575,-0.454602843714802,
1.715480776583));
#21773=CARTESIAN_POINT('Ctrl Pts',(1.46714441944577,-0.377981286365637,
1.81902921434248));
#21774=CARTESIAN_POINT('Ctrl Pts',(1.5699559447672,-0.259766273896474,1.90869858745619));
#21775=CARTESIAN_POINT('',(1.81394816223928,-0.428377445609995,1.63615580822897));
#21776=CARTESIAN_POINT('Ctrl Pts',(1.81394816223928,-0.428377445609995,
1.63615580822897));
#21777=CARTESIAN_POINT('Ctrl Pts',(1.79068402602087,-0.396788109812435,
1.66605750085059));
#21778=CARTESIAN_POINT('Ctrl Pts',(1.76065343036505,-0.361451075078504,
1.70278841264342));
#21779=CARTESIAN_POINT('Ctrl Pts',(1.70449155357827,-0.313194031324451,
1.76702045133065));
#21780=CARTESIAN_POINT('Ctrl Pts',(1.67910176739992,-0.293827753703524,
1.79540516147607));
#21781=CARTESIAN_POINT('Ctrl Pts',(1.63136425547036,-0.270592580621385,
1.84635863460718));
#21782=CARTESIAN_POINT('Ctrl Pts',(1.60535049511978,-0.261679155446849,
1.87346655258888));
#21783=CARTESIAN_POINT('Ctrl Pts',(1.5699559447672,-0.259766273896474,1.90869858745619));
#21784=CARTESIAN_POINT('Ctrl Pts',(1.08521613661244,-0.642908916934723,
1.10727038327973));
#21785=CARTESIAN_POINT('Ctrl Pts',(1.16760035714813,-0.668710261798003,
1.18103565901042));
#21786=CARTESIAN_POINT('Ctrl Pts',(1.25518160519556,-0.681355585835302,
1.25302429310885));
#21787=CARTESIAN_POINT('Ctrl Pts',(1.44098614169382,-0.665371573463992,
1.39260788389872));
#21788=CARTESIAN_POINT('Ctrl Pts',(1.53389259595497,-0.635301149560131,
1.45574709063856));
#21789=CARTESIAN_POINT('Ctrl Pts',(1.69239761845937,-0.541698310562567,
1.55895701082587));
#21790=CARTESIAN_POINT('Ctrl Pts',(1.75616935678546,-0.489122861296313,
1.59904902099409));
#21791=CARTESIAN_POINT('Ctrl Pts',(1.81394816223928,-0.428377445609995,
1.63615580822897));
#21792=CARTESIAN_POINT('Ctrl Pts',(1.21487793679797,-0.362330138275323,
1.10149705943221));
#21793=CARTESIAN_POINT('Ctrl Pts',(1.48329895916361,-0.383459937582893,
1.31979778023781));
#21794=CARTESIAN_POINT('Ctrl Pts',(1.70227260218966,-0.249644960941914,
1.49880741124996));
#21795=CARTESIAN_POINT('Ctrl Pts',(1.87179886587611,0.0391147916476142,
1.63852595246867));
#21796=CARTESIAN_POINT('Ctrl Pts',(1.18333690797345,-0.373447482460584,
1.12583385309083));
#21797=CARTESIAN_POINT('Ctrl Pts',(1.44573672483852,-0.398305182537799,
1.34892944774501));
#21798=CARTESIAN_POINT('Ctrl Pts',(1.66212671668267,-0.270675994878902,
1.5318660237053));
#21799=CARTESIAN_POINT('Ctrl Pts',(1.83255854794259,0.00930365130125684,
1.67464838892921));
#21800=CARTESIAN_POINT('Ctrl Pts',(1.13169790455625,-0.386758017000778,
1.16764044916318));
#21801=CARTESIAN_POINT('Ctrl Pts',(1.38402127269754,-0.416680587119745,
1.39897336709085));
#21802=CARTESIAN_POINT('Ctrl Pts',(1.59542335194445,-0.298670375694656,
1.58871211231351));
#21803=CARTESIAN_POINT('Ctrl Pts',(1.76604232095017,-0.0327265383253196,
1.73676275687621));
#21804=CARTESIAN_POINT('Ctrl Pts',(1.06341115236232,-0.39167174183756,1.22801607619329));
#21805=CARTESIAN_POINT('Ctrl Pts',(1.30168216224369,-0.425665904909547,
1.47139032317727));
#21806=CARTESIAN_POINT('Ctrl Pts',(1.50457544636212,-0.318647566754319,
1.67096220367118));
#21807=CARTESIAN_POINT('Ctrl Pts',(1.67209124376879,-0.0706042875438403,
1.82672793765153));
#21808=CARTESIAN_POINT('Ctrl Pts',(1.0286884268729,-0.38218165487343,1.263527751515));
#21809=CARTESIAN_POINT('Ctrl Pts',(1.25929056133869,-0.415770412604396,
1.51397381108002));
#21810=CARTESIAN_POINT('Ctrl Pts',(1.45588630034146,-0.312692596804321,
1.71945276482244));
#21811=CARTESIAN_POINT('Ctrl Pts',(1.61878272768802,-0.0729619965738721,
1.87976043671971));
#21812=CARTESIAN_POINT('Ctrl Pts',(1.01098164381094,-0.373486051297297,
1.28318517919159));
#21813=CARTESIAN_POINT('Ctrl Pts',(1.23750736860246,-0.406026489679721,
1.53754499301511));
#21814=CARTESIAN_POINT('Ctrl Pts',(1.43052436008973,-0.304436793685253,
1.74612783237316));
#21815=CARTESIAN_POINT('Ctrl Pts',(1.59003261827274,-0.0687169633138944,
1.90893369726573));
#21816=CARTESIAN_POINT('',(1.20742290720348,-0.364905277844141,1.10727038327973));
#21817=CARTESIAN_POINT('',(1.01462217612883,-0.373997862975654,1.28727233489076));
#21818=CARTESIAN_POINT('Ctrl Pts',(1.20742290720348,-0.364905277844141,
1.10727038327973));
#21819=CARTESIAN_POINT('Ctrl Pts',(1.18311862080933,-0.373615945090665,
1.12801545944046));
#21820=CARTESIAN_POINT('Ctrl Pts',(1.15609247800026,-0.381365818655255,
1.15133239961427));
#21821=CARTESIAN_POINT('Ctrl Pts',(1.10715678825458,-0.389206856698246,
1.19509600545485));
#21822=CARTESIAN_POINT('Ctrl Pts',(1.08733497046196,-0.390682503085345,
1.2132474061745));
#21823=CARTESIAN_POINT('Ctrl Pts',(1.05408067239119,-0.388091095569738,
1.24538218411127));
#21824=CARTESIAN_POINT('Ctrl Pts',(1.03595219175474,-0.384447468688916,
1.26364457695044));
#21825=CARTESIAN_POINT('Ctrl Pts',(1.01462217612883,-0.373997862975654,
1.28727233489076));
#21826=CARTESIAN_POINT('',(1.86363850813291,0.0276890267571665,1.63615580822897));
#21827=CARTESIAN_POINT('Ctrl Pts',(1.86363850813291,0.0276890267571664,
1.63615580822897));
#21828=CARTESIAN_POINT('Ctrl Pts',(1.80655480211395,-0.0698239366990066,
1.58477934055781));
#21829=CARTESIAN_POINT('Ctrl Pts',(1.74187241700953,-0.148691945288574,
1.53343685544651));
#21830=CARTESIAN_POINT('Ctrl Pts',(1.59669345888589,-0.274785130849277,
1.42076782591239));
#21831=CARTESIAN_POINT('Ctrl Pts',(1.51444831269985,-0.320436333138584,
1.35830292226017));
#21832=CARTESIAN_POINT('Ctrl Pts',(1.35321270714141,-0.366271065016131,
1.23020598103184));
#21833=CARTESIAN_POINT('Ctrl Pts',(1.2795761902763,-0.371649422530894,1.1696137009149));
#21834=CARTESIAN_POINT('Ctrl Pts',(1.20742290720348,-0.364905277844141,
1.10727038327973));
#21835=CARTESIAN_POINT('',(1.58980227845634,-0.0690572297370891,1.90869858745619));
#21836=CARTESIAN_POINT('Ctrl Pts',(1.58980227845634,-0.0690572297370894,
1.90869858745619));
#21837=CARTESIAN_POINT('Ctrl Pts',(1.63853765425277,-0.0758898445998981,
1.85971261137246));
#21838=CARTESIAN_POINT('Ctrl Pts',(1.67950604280849,-0.0682369940313469,
1.81924683990323));
#21839=CARTESIAN_POINT('Ctrl Pts',(1.7703562129981,-0.0309159708914552,
1.7294679192124));
#21840=CARTESIAN_POINT('Ctrl Pts',(1.81575345115033,-0.00571744860871286,
1.68453186312949));
#21841=CARTESIAN_POINT('Ctrl Pts',(1.86363850813291,0.0276890267571661,
1.63615580822897));
#21842=CARTESIAN_POINT('Ctrl Pts',(1.01462217612883,-0.373997862975654,
1.28727233489076));
#21843=CARTESIAN_POINT('Ctrl Pts',(1.11493412912611,-0.387792676785359,
1.39987124007464));
#21844=CARTESIAN_POINT('Ctrl Pts',(1.20865423507634,-0.375201374409042,
1.50346488650363));
#21845=CARTESIAN_POINT('Ctrl Pts',(1.40394856048621,-0.287835131123856,
1.715480776583));
#21846=CARTESIAN_POINT('Ctrl Pts',(1.50195515531182,-0.198779555753985,
1.81902921434248));
#21847=CARTESIAN_POINT('Ctrl Pts',(1.58980227845634,-0.0690572297370891,
1.90869858745619));
#21848=CARTESIAN_POINT('Ctrl Pts',(1.01462217612883,-0.373997862975654,
1.28727233489076));
#21849=CARTESIAN_POINT('Ctrl Pts',(1.24016643693111,-0.405014516431692,
1.54044292999952));
#21850=CARTESIAN_POINT('Ctrl Pts',(1.43238606966553,-0.302637979515068,
1.74808806061869));
#21851=CARTESIAN_POINT('Ctrl Pts',(1.59128107433209,-0.0668682522257824,
1.91020772674828));
#21852=CARTESIAN_POINT('Ctrl Pts',(0.997173125995706,-0.413770122869549,
1.28727233489076));
#21853=CARTESIAN_POINT('Ctrl Pts',(1.22092814469495,-0.453754022216744,
1.54044292999952));
#21854=CARTESIAN_POINT('Ctrl Pts',(1.41678703930426,-0.359331486839601,
1.74808806061869));
#21855=CARTESIAN_POINT('Ctrl Pts',(1.58474980982363,-0.130502516738118,
1.91020772674828));
#21856=CARTESIAN_POINT('Ctrl Pts',(0.979724075862581,-0.453542382763444,
1.28727233489076));
#21857=CARTESIAN_POINT('Ctrl Pts',(1.2016898524588,-0.502493528001797,1.54044292999952));
#21858=CARTESIAN_POINT('Ctrl Pts',(1.40118800894299,-0.416024994164134,
1.74808806061869));
#21859=CARTESIAN_POINT('Ctrl Pts',(1.57821854531517,-0.194136781250453,
1.91020772674828));
#21860=CARTESIAN_POINT('Ctrl Pts',(0.962275025729455,-0.493314642657339,
1.28727233489076));
#21861=CARTESIAN_POINT('Ctrl Pts',(1.18245156022264,-0.55123303378685,1.54044292999952));
#21862=CARTESIAN_POINT('Ctrl Pts',(1.38558897858172,-0.472718501488667,
1.74808806061869));
#21863=CARTESIAN_POINT('Ctrl Pts',(1.5716872808067,-0.257771045762789,1.91020772674828));
#21864=CARTESIAN_POINT('Ctrl Pts',(1.01462217612883,-0.373997862975654,
1.28727233489076));
#21865=CARTESIAN_POINT('Ctrl Pts',(1.00648281422349,-0.394056488869181,
1.28797191329047));
#21866=CARTESIAN_POINT('Ctrl Pts',(0.998068152324092,-0.414003503730721,
1.28831907556383));
#21867=CARTESIAN_POINT('Ctrl Pts',(0.989370462098315,-0.433838594404394,
1.288319084765));
#21868=CARTESIAN_POINT('Ctrl Pts',(0.98061834720741,-0.453797800577661,
1.28831909402374));
#21869=CARTESIAN_POINT('Ctrl Pts',(0.97158845574471,-0.473623504353524,
1.28796761487395));
#21870=CARTESIAN_POINT('Ctrl Pts',(0.962275025729455,-0.493314642657339,
1.28727233489076));
#21871=CARTESIAN_POINT('Ctrl Pts',(1.5699559447672,-0.259766273896474,1.90869858745619));
#21872=CARTESIAN_POINT('Ctrl Pts',(1.57432246394088,-0.227349477989724,
1.90968240330487));
#21873=CARTESIAN_POINT('Ctrl Pts',(1.57814313696878,-0.194870259405019,
1.91020759224355));
#21874=CARTESIAN_POINT('Ctrl Pts',(1.58148345331813,-0.162326115709102,
1.91020766105751));
#21875=CARTESIAN_POINT('Ctrl Pts',(1.5846721664331,-0.131259016977809,1.91020772674828));
#21876=CARTESIAN_POINT('Ctrl Pts',(1.58741938775354,-0.100166338107427,
1.90972920064616));
#21877=CARTESIAN_POINT('Ctrl Pts',(1.58980227845634,-0.0690572297370893,
1.90869858745619));
#21878=CARTESIAN_POINT('Origin',(0.,0.,1.86807790411448));
#21879=CARTESIAN_POINT('',(-1.4,-1.71450551880629E-16,2.1));
#21880=CARTESIAN_POINT('Origin',(0.,0.,2.1));
#21881=CARTESIAN_POINT('',(-1.82153560297087,-2.51062254834063E-10,1.67846439702913));
#21882=CARTESIAN_POINT('',(-1.63192209588552,-1.99852817118404E-16,1.86807790411448));
#21883=CARTESIAN_POINT('',(-1.86363850813291,-0.0276890267571664,1.63615580822897));
#21884=CARTESIAN_POINT('Ctrl Pts',(-1.82153560297087,-5.02124314349928E-10,
1.67846439702913));
#21885=CARTESIAN_POINT('Ctrl Pts',(-1.835325320101,-0.00850724271337055,
1.66467467989666));
#21886=CARTESIAN_POINT('Ctrl Pts',(-1.84937147874757,-0.017735792998272,
1.65056912712851));
#21887=CARTESIAN_POINT('Ctrl Pts',(-1.86363850813291,-0.027689026757167,
1.63615580822897));
#21888=CARTESIAN_POINT('',(-1.85754313061971,-0.153129647965885,1.63615580822897));
#21889=CARTESIAN_POINT('Origin',(0.,0.,1.63615580822897));
#21890=CARTESIAN_POINT('',(-1.57338902476662,-0.238090659850088,1.90869858745619));
#21891=CARTESIAN_POINT('Ctrl Pts',(-1.85754313061971,-0.153129647965885,
1.63615580822897));
#21892=CARTESIAN_POINT('Ctrl Pts',(-1.8208638312973,-0.179418518304102,
1.67055126645182));
#21893=CARTESIAN_POINT('Ctrl Pts',(-1.77686224462366,-0.205674380666754,
1.71144473817108));
#21894=CARTESIAN_POINT('Ctrl Pts',(-1.68888826787379,-0.239335933327674,
1.79435460643495));
#21895=CARTESIAN_POINT('Ctrl Pts',(-1.6630238425637,-0.243149658729552,
1.81929762514764));
#21896=CARTESIAN_POINT('Ctrl Pts',(-1.63091267750169,-0.246644834768741,
1.85055034165243));
#21897=CARTESIAN_POINT('Ctrl Pts',(-1.60540976577649,-0.246614602123327,
1.87576293296796));
#21898=CARTESIAN_POINT('Ctrl Pts',(-1.57338902476662,-0.238090659850087,
1.90869858745619));
#21899=CARTESIAN_POINT('',(-1.53333167412,-0.425598593400271,1.90869858745619));
#21900=CARTESIAN_POINT('Ctrl Pts',(-1.57338902476662,-0.238090659850087,
1.90869858745619));
#21901=CARTESIAN_POINT('Ctrl Pts',(-1.56752449044192,-0.270270193465538,
1.90968240330487));
#21902=CARTESIAN_POINT('Ctrl Pts',(-1.56112153591504,-0.30234041884027,
1.91020759224355));
#21903=CARTESIAN_POINT('Ctrl Pts',(-1.55424167207615,-0.334323953288057,
1.91020766105751));
#21904=CARTESIAN_POINT('Ctrl Pts',(-1.54767405698886,-0.364855886521523,
1.91020772674828));
#21905=CARTESIAN_POINT('Ctrl Pts',(-1.54067865355577,-0.395275719445611,
1.90972920064616));
#21906=CARTESIAN_POINT('Ctrl Pts',(-1.53333167412,-0.425598593400271,1.90869858745619));
#21907=CARTESIAN_POINT('',(-1.76386916735272,-0.602229799711917,1.63615580822897));
#21908=CARTESIAN_POINT('Ctrl Pts',(-1.53333167412,-0.425598593400271,1.90869858745619));
#21909=CARTESIAN_POINT('Ctrl Pts',(-1.58179316495641,-0.434160449860449,
1.85971261136993));
#21910=CARTESIAN_POINT('Ctrl Pts',(-1.61839155697287,-0.454098671559182,
1.81924683990076));
#21911=CARTESIAN_POINT('Ctrl Pts',(-1.69326237295061,-0.517667320349936,
1.72946791919794));
#21912=CARTESIAN_POINT('Ctrl Pts',(-1.72865094049847,-0.55566105726035,
1.68453186311304));
#21913=CARTESIAN_POINT('Ctrl Pts',(-1.76386916735272,-0.602229799711918,
1.63615580822897));
#21914=CARTESIAN_POINT('',(-1.71930883511106,-0.71964734468187,1.63615580822897));
#21915=CARTESIAN_POINT('Origin',(0.,0.,1.63615580822897));
#21916=CARTESIAN_POINT('',(-1.42280782457595,-0.71264162093535,1.90869858745619));
#21917=CARTESIAN_POINT('Ctrl Pts',(-1.71930883511106,-0.71964734468187,
1.63615580822897));
#21918=CARTESIAN_POINT('Ctrl Pts',(-1.68192000782792,-0.731529338010255,
1.66605750085977));
#21919=CARTESIAN_POINT('Ctrl Pts',(-1.6368541577183,-0.742466058393773,
1.70278841265036));
#21920=CARTESIAN_POINT('Ctrl Pts',(-1.56305346633165,-0.748495703972133,
1.76702045133087));
#21921=CARTESIAN_POINT('Ctrl Pts',(-1.53112948545226,-0.749239609810652,
1.7954051614765));
#21922=CARTESIAN_POINT('Ctrl Pts',(-1.47885173495873,-0.739977854207805,
1.84635863460877));
#21923=CARTESIAN_POINT('Ctrl Pts',(-1.45256698088295,-0.73189846196087,
1.87346655259029));
#21924=CARTESIAN_POINT('Ctrl Pts',(-1.42280782457595,-0.71264162093535,
1.90869858745619));
#21925=CARTESIAN_POINT('',(-1.32676788217082,-0.878593860895847,1.90869858745619));
#21926=CARTESIAN_POINT('Ctrl Pts',(-1.42280782457595,-0.71264162093535,
1.90869858745619));
#21927=CARTESIAN_POINT('Ctrl Pts',(-1.40728629823317,-0.741433935301229,
1.90968240330487));
#21928=CARTESIAN_POINT('Ctrl Pts',(-1.39128648195262,-0.769955910359912,
1.91020759224355));
#21929=CARTESIAN_POINT('Ctrl Pts',(-1.37485988693288,-0.79824806436543,
1.91020766105751));
#21930=CARTESIAN_POINT('Ctrl Pts',(-1.3591788275673,-0.825256153747753,
1.91020772674828));
#21931=CARTESIAN_POINT('Ctrl Pts',(-1.34312555820857,-0.852025435531464,
1.90972920064616));
#21932=CARTESIAN_POINT('Ctrl Pts',(-1.32676788217082,-0.878593860895846,
1.90869858745619));
#21933=CARTESIAN_POINT('',(-1.4914400228729,-1.11782012388912,1.63615580822897));
#21934=CARTESIAN_POINT('Ctrl Pts',(-1.32676788217082,-0.878593860895847,
1.90869858745619));
#21935=CARTESIAN_POINT('Ctrl Pts',(-1.37021173966974,-0.901712094514641,
1.85971261137088));
#21936=CARTESIAN_POINT('Ctrl Pts',(-1.39885762954068,-0.931983995284014,
1.81924683990171));
#21937=CARTESIAN_POINT('Ctrl Pts',(-1.45042021416875,-1.01557772746493,
1.72946791920256));
#21938=CARTESIAN_POINT('Ctrl Pts',(-1.47233603155308,-1.06264758730959,
1.68453186311793));
#21939=CARTESIAN_POINT('Ctrl Pts',(-1.4914400228729,-1.11782012388912,1.63615580822897));
#21940=CARTESIAN_POINT('',(-1.4127766116927,-1.21572094522251,1.63615580822897));
#21941=CARTESIAN_POINT('Origin',(0.,0.,1.63615580822897));
#21942=CARTESIAN_POINT('',(-1.13295228123076,-1.11743425489732,1.90869858745619));
#21943=CARTESIAN_POINT('Ctrl Pts',(-1.4127766116927,-1.21572094522251,1.63615580822897));
#21944=CARTESIAN_POINT('Ctrl Pts',(-1.3735459860182,-1.2154676093739,1.66605750084812));
#21945=CARTESIAN_POINT('Ctrl Pts',(-1.32730618314253,-1.21194293501399,
1.70278841264146));
#21946=CARTESIAN_POINT('Ctrl Pts',(-1.25525429172787,-1.19487180089464,
1.76702045133136));
#21947=CARTESIAN_POINT('Ctrl Pts',(-1.2246629021408,-1.18571424477025,1.79540516147636));
#21948=CARTESIAN_POINT('Ctrl Pts',(-1.17780584675887,-1.16075107842331,
1.84635863460519));
#21949=CARTESIAN_POINT('Ctrl Pts',(-1.15530422962322,-1.14494468407762,
1.87346655258698));
#21950=CARTESIAN_POINT('Ctrl Pts',(-1.13295228123076,-1.11743425489732,
1.90869858745619));
#21951=CARTESIAN_POINT('',(-0.990330805779366,-1.24558623976355,1.90869858745619));
#21952=CARTESIAN_POINT('Ctrl Pts',(-1.13295228123076,-1.11743425489732,
1.90869858745619));
#21953=CARTESIAN_POINT('Ctrl Pts',(-1.10929311801315,-1.14002095767567,
1.90968240330488));
#21954=CARTESIAN_POINT('Ctrl Pts',(-1.08526261347374,-1.16220275277526,
1.91020759224355));
#21955=CARTESIAN_POINT('Ctrl Pts',(-1.0608972368445,-1.18403409318141,1.91020766105751));
#21956=CARTESIAN_POINT('Ctrl Pts',(-1.03763770454778,-1.20487459874735,
1.91020772674828));
#21957=CARTESIAN_POINT('Ctrl Pts',(-1.01409797511791,-1.22537296557718,
1.90972920064616));
#21958=CARTESIAN_POINT('Ctrl Pts',(-0.990330805779366,-1.24558623976355,
1.90869858745619));
#21959=CARTESIAN_POINT('',(-1.07301833748062,-1.52399042602929,1.63615580822897));
#21960=CARTESIAN_POINT('Ctrl Pts',(-0.990330805779367,-1.24558623976355,
1.90869858745619));
#21961=CARTESIAN_POINT('Ctrl Pts',(-1.02450444247791,-1.28099787675963,
1.85971261137182));
#21962=CARTESIAN_POINT('Ctrl Pts',(-1.04239377091547,-1.31864023203577,
1.81924683990262));
#21963=CARTESIAN_POINT('Ctrl Pts',(-1.06560081914983,-1.4140763106475,1.72946791922643));
#21964=CARTESIAN_POINT('Ctrl Pts',(-1.07189861347384,-1.465614767582,1.6845318631466));
#21965=CARTESIAN_POINT('Ctrl Pts',(-1.07301833748062,-1.52399042602929,
1.63615580822897));
#21966=CARTESIAN_POINT('',(-0.967951970128401,-1.59279130921887,1.63615580822897));
#21967=CARTESIAN_POINT('Origin',(0.,0.,1.63615580822897));
#21968=CARTESIAN_POINT('',(-0.732195474855993,-1.41284463836769,1.90869858745619));
#21969=CARTESIAN_POINT('Ctrl Pts',(-0.967951970128401,-1.59279130921887,
1.63615580822897));
#21970=CARTESIAN_POINT('Ctrl Pts',(-0.930719713024342,-1.58042744247569,
1.66605750084852));
#21971=CARTESIAN_POINT('Ctrl Pts',(-0.88783223146424,-1.56278639305271,
1.7027884126418));
#21972=CARTESIAN_POINT('Ctrl Pts',(-0.824582081179338,-1.52428552078414,
1.76702045133143));
#21973=CARTESIAN_POINT('Ctrl Pts',(-0.798317781239416,-1.50612290809472,
1.79540516147644));
#21974=CARTESIAN_POINT('Ctrl Pts',(-0.761468116016933,-1.46790189965195,
1.84635863460764));
#21975=CARTESIAN_POINT('Ctrl Pts',(-0.744952250886494,-1.44591574321431,
1.87346655258914));
#21976=CARTESIAN_POINT('Ctrl Pts',(-0.732195474855993,-1.41284463836769,
1.90869858745619));
#21977=CARTESIAN_POINT('',(-0.55695325007777,-1.49065195897357,1.90869858745619));
#21978=CARTESIAN_POINT('Ctrl Pts',(-0.732195474855993,-1.41284463836769,
1.90869858745619));
#21979=CARTESIAN_POINT('Ctrl Pts',(-0.702714598502394,-1.42701478571972,
1.90968240330488));
#21980=CARTESIAN_POINT('Ctrl Pts',(-0.673005678918811,-1.44068509220623,
1.91020759224355));
#21981=CARTESIAN_POINT('Ctrl Pts',(-0.643086573508102,-1.45391861530618,
1.91020766105751));
#21982=CARTESIAN_POINT('Ctrl Pts',(-0.614525373360046,-1.46655152316666,
1.91020772674828));
#21983=CARTESIAN_POINT('Ctrl Pts',(-0.585803416586614,-1.47877245207676,
1.90972920064616));
#21984=CARTESIAN_POINT('Ctrl Pts',(-0.556953250077771,-1.49065195897357,
1.90869858745619));
#21985=CARTESIAN_POINT('',(-0.549562141057369,-1.78098192700405,1.63615580822897));
#21986=CARTESIAN_POINT('Ctrl Pts',(-0.55695325007777,-1.49065195897357,
1.90869858745619));
#21987=CARTESIAN_POINT('Ctrl Pts',(-0.578511512315346,-1.53489066159152,
1.85971261137103));
#21988=CARTESIAN_POINT('Ctrl Pts',(-0.583893147208912,-1.57621877537089,
1.81924683990186));
#21989=CARTESIAN_POINT('Ctrl Pts',(-0.576472991487369,-1.67415525213672,
1.7294679192084));
#21990=CARTESIAN_POINT('Ctrl Pts',(-0.566536290754651,-1.72511736292283,
1.68453186312477));
#21991=CARTESIAN_POINT('Ctrl Pts',(-0.549562141057369,-1.78098192700405,
1.63615580822897));
#21992=CARTESIAN_POINT('',(-0.428377445609995,-1.81394816223928,1.63615580822897));
#21993=CARTESIAN_POINT('Origin',(0.,0.,1.63615580822897));
#21994=CARTESIAN_POINT('',(-0.259766273896474,-1.5699559447672,1.90869858745619));
#21995=CARTESIAN_POINT('Ctrl Pts',(-0.428377445609995,-1.81394816223928,
1.63615580822897));
#21996=CARTESIAN_POINT('Ctrl Pts',(-0.396788109819453,-1.79068402602605,
1.66605750084394));
#21997=CARTESIAN_POINT('Ctrl Pts',(-0.361451075082306,-1.76065343036948,
1.70278841263835));
#21998=CARTESIAN_POINT('Ctrl Pts',(-0.313194031324859,-1.70449155357874,
1.76702045133011));
#21999=CARTESIAN_POINT('Ctrl Pts',(-0.29382775370378,-1.67910176740044,
1.79540516147552));
#22000=CARTESIAN_POINT('Ctrl Pts',(-0.270592580621278,-1.63136425547015,
1.84635863460741));
#22001=CARTESIAN_POINT('Ctrl Pts',(-0.261679155446836,-1.60535049511953,
1.87346655258912));
#22002=CARTESIAN_POINT('Ctrl Pts',(-0.259766273896474,-1.5699559447672,
1.90869858745619));
#22003=CARTESIAN_POINT('',(-0.0690572297370887,-1.58980227845634,1.90869858745619));
#22004=CARTESIAN_POINT('Ctrl Pts',(-0.259766273896473,-1.5699559447672,
1.90869858745619));
#22005=CARTESIAN_POINT('Ctrl Pts',(-0.227349477989679,-1.57432246394089,
1.90968240330488));
#22006=CARTESIAN_POINT('Ctrl Pts',(-0.194870259404996,-1.57814313696878,
1.91020759224355));
#22007=CARTESIAN_POINT('Ctrl Pts',(-0.162326115709102,-1.58148345331813,
1.91020766105751));
#22008=CARTESIAN_POINT('Ctrl Pts',(-0.131259016977817,-1.5846721664331,
1.91020772674828));
#22009=CARTESIAN_POINT('Ctrl Pts',(-0.100166338107431,-1.58741938775353,
1.90972920064616));
#22010=CARTESIAN_POINT('Ctrl Pts',(-0.0690572297370894,-1.58980227845634,
1.90869858745619));
#22011=CARTESIAN_POINT('',(0.0276890267571667,-1.86363850813291,1.63615580822897));
#22012=CARTESIAN_POINT('Ctrl Pts',(-0.0690572297370892,-1.58980227845634,
1.90869858745619));
#22013=CARTESIAN_POINT('Ctrl Pts',(-0.0758898445996493,-1.63853765425097,
1.85971261137426));
#22014=CARTESIAN_POINT('Ctrl Pts',(-0.0682369940319697,-1.6795060428066,
1.81924683990509));
#22015=CARTESIAN_POINT('Ctrl Pts',(-0.0309159709011246,-1.77035621297488,
1.72946791923535));
#22016=CARTESIAN_POINT('Ctrl Pts',(-0.00571744862659264,-1.8157534511247,
1.68453186315538));
#22017=CARTESIAN_POINT('Ctrl Pts',(0.0276890267571667,-1.86363850813291,
1.63615580822897));
#22018=CARTESIAN_POINT('',(0.153129647965884,-1.85754313061971,1.63615580822897));
#22019=CARTESIAN_POINT('Origin',(0.,0.,1.63615580822897));
#22020=CARTESIAN_POINT('',(0.238090659850087,-1.57338902476662,1.90869858745619));
#22021=CARTESIAN_POINT('Ctrl Pts',(0.153129647965884,-1.85754313061971,
1.63615580822897));
#22022=CARTESIAN_POINT('Ctrl Pts',(0.17941851828628,-1.82086383132218,1.67055126642849));
#22023=CARTESIAN_POINT('Ctrl Pts',(0.205674380657903,-1.77686224464677,
1.7114447381493));
#22024=CARTESIAN_POINT('Ctrl Pts',(0.23933593332684,-1.68888826787598,1.79435460643288));
#22025=CARTESIAN_POINT('Ctrl Pts',(0.243149658729243,-1.66302384256654,
1.81929762514487));
#22026=CARTESIAN_POINT('Ctrl Pts',(0.246644834768774,-1.63091267750138,
1.85055034165273));
#22027=CARTESIAN_POINT('Ctrl Pts',(0.246614602123246,-1.60540976577619,
1.87576293296827));
#22028=CARTESIAN_POINT('Ctrl Pts',(0.238090659850087,-1.57338902476662,
1.90869858745619));
#22029=CARTESIAN_POINT('',(0.425598593400271,-1.53333167412,1.90869858745619));
#22030=CARTESIAN_POINT('Ctrl Pts',(0.238090659850087,-1.57338902476662,
1.90869858745619));
#22031=CARTESIAN_POINT('Ctrl Pts',(0.270270193465529,-1.56752449044192,
1.90968240330487));
#22032=CARTESIAN_POINT('Ctrl Pts',(0.302340418840266,-1.56112153591504,
1.91020759224355));
#22033=CARTESIAN_POINT('Ctrl Pts',(0.334323953288058,-1.55424167207615,
1.91020766105751));
#22034=CARTESIAN_POINT('Ctrl Pts',(0.364855886521546,-1.54767405698885,
1.91020772674828));
#22035=CARTESIAN_POINT('Ctrl Pts',(0.395275719445622,-1.54067865355577,
1.90972920064616));
#22036=CARTESIAN_POINT('Ctrl Pts',(0.425598593400271,-1.53333167412,1.90869858745619));
#22037=CARTESIAN_POINT('',(0.602229799711917,-1.76386916735272,1.63615580822897));
#22038=CARTESIAN_POINT('Ctrl Pts',(0.425598593400271,-1.53333167412,1.90869858745619));
#22039=CARTESIAN_POINT('Ctrl Pts',(0.434160449860198,-1.58179316495496,
1.8597126113714));
#22040=CARTESIAN_POINT('Ctrl Pts',(0.454098671558146,-1.61839155697167,
1.8192468399022));
#22041=CARTESIAN_POINT('Ctrl Pts',(0.517667320342287,-1.69326237294158,
1.72946791920875));
#22042=CARTESIAN_POINT('Ctrl Pts',(0.555661057248714,-1.72865094048965,
1.68453186312515));
#22043=CARTESIAN_POINT('Ctrl Pts',(0.602229799711917,-1.76386916735272,
1.63615580822897));
#22044=CARTESIAN_POINT('',(0.71964734468187,-1.71930883511106,1.63615580822897));
#22045=CARTESIAN_POINT('Origin',(0.,0.,1.63615580822897));
#22046=CARTESIAN_POINT('',(0.71264162093535,-1.42280782457595,1.90869858745619));
#22047=CARTESIAN_POINT('Ctrl Pts',(0.71964734468187,-1.71930883511106,1.63615580822897));
#22048=CARTESIAN_POINT('Ctrl Pts',(0.731529338009191,-1.68192000783126,
1.6660575008571));
#22049=CARTESIAN_POINT('Ctrl Pts',(0.742466058393583,-1.63685415772067,
1.70278841264829));
#22050=CARTESIAN_POINT('Ctrl Pts',(0.7484957039722,-1.56305346633081,1.76702045133161));
#22051=CARTESIAN_POINT('Ctrl Pts',(0.749239609810595,-1.53112948545192,
1.79540516147683));
#22052=CARTESIAN_POINT('Ctrl Pts',(0.739977854208178,-1.47885173496085,
1.84635863460671));
#22053=CARTESIAN_POINT('Ctrl Pts',(0.73189846196194,-1.4525669808846,1.87346655258834));
#22054=CARTESIAN_POINT('Ctrl Pts',(0.71264162093535,-1.42280782457595,1.90869858745619));
#22055=CARTESIAN_POINT('',(0.878593860895847,-1.32676788217082,1.90869858745619));
#22056=CARTESIAN_POINT('Ctrl Pts',(0.712641620935351,-1.42280782457595,
1.90869858745619));
#22057=CARTESIAN_POINT('Ctrl Pts',(0.741433935301239,-1.40728629823317,
1.90968240330488));
#22058=CARTESIAN_POINT('Ctrl Pts',(0.769955910359916,-1.39128648195261,
1.91020759224355));
#22059=CARTESIAN_POINT('Ctrl Pts',(0.798248064365429,-1.37485988693288,
1.91020766105751));
#22060=CARTESIAN_POINT('Ctrl Pts',(0.825256153747754,-1.3591788275673,1.91020772674828));
#22061=CARTESIAN_POINT('Ctrl Pts',(0.852025435531465,-1.34312555820857,
1.90972920064616));
#22062=CARTESIAN_POINT('Ctrl Pts',(0.878593860895846,-1.32676788217082,
1.90869858745619));
#22063=CARTESIAN_POINT('',(1.11782012388912,-1.4914400228729,1.63615580822897));
#22064=CARTESIAN_POINT('Ctrl Pts',(0.878593860895847,-1.32676788217082,
1.90869858745619));
#22065=CARTESIAN_POINT('Ctrl Pts',(0.901712094513363,-1.37021173966734,
1.85971261137359));
#22066=CARTESIAN_POINT('Ctrl Pts',(0.9319839952815,-1.39885762953914,1.8192468399044));
#22067=CARTESIAN_POINT('Ctrl Pts',(1.01557772744379,-1.45042021415571,1.72946791922527));
#22068=CARTESIAN_POINT('Ctrl Pts',(1.06264758728011,-1.47233603154289,1.68453186314377));
#22069=CARTESIAN_POINT('Ctrl Pts',(1.11782012388912,-1.4914400228729,1.63615580822897));
#22070=CARTESIAN_POINT('',(1.21572094522251,-1.4127766116927,1.63615580822897));
#22071=CARTESIAN_POINT('Origin',(0.,0.,1.63615580822897));
#22072=CARTESIAN_POINT('',(1.11743425489732,-1.13295228123076,1.90869858745619));
#22073=CARTESIAN_POINT('Ctrl Pts',(1.21572094522251,-1.4127766116927,1.63615580822897));
#22074=CARTESIAN_POINT('Ctrl Pts',(1.21546760937391,-1.37354598601756,1.6660575008486));
#22075=CARTESIAN_POINT('Ctrl Pts',(1.21194293501389,-1.3273061831421,1.70278841264184));
#22076=CARTESIAN_POINT('Ctrl Pts',(1.19487180089496,-1.25525429172921,1.76702045133017));
#22077=CARTESIAN_POINT('Ctrl Pts',(1.18571424477058,-1.22466290214144,1.79540516147567));
#22078=CARTESIAN_POINT('Ctrl Pts',(1.16075107842279,-1.17780584675786,1.84635863460628));
#22079=CARTESIAN_POINT('Ctrl Pts',(1.14494468407672,-1.15530422962249,1.87346655258813));
#22080=CARTESIAN_POINT('Ctrl Pts',(1.11743425489732,-1.13295228123076,1.90869858745619));
#22081=CARTESIAN_POINT('',(1.24558623976355,-0.990330805779367,1.90869858745619));
#22082=CARTESIAN_POINT('Ctrl Pts',(1.11743425489732,-1.13295228123076,1.90869858745619));
#22083=CARTESIAN_POINT('Ctrl Pts',(1.14002095767566,-1.10929311801316,1.90968240330487));
#22084=CARTESIAN_POINT('Ctrl Pts',(1.16220275277526,-1.08526261347375,1.91020759224355));
#22085=CARTESIAN_POINT('Ctrl Pts',(1.18403409318141,-1.0608972368445,1.91020766105751));
#22086=CARTESIAN_POINT('Ctrl Pts',(1.20487459874738,-1.03763770454774,1.91020772674828));
#22087=CARTESIAN_POINT('Ctrl Pts',(1.2253729655772,-1.01409797511789,1.90972920064616));
#22088=CARTESIAN_POINT('Ctrl Pts',(1.24558623976355,-0.990330805779366,
1.90869858745619));
#22089=CARTESIAN_POINT('',(1.52399042602929,-1.07301833748062,1.63615580822897));
#22090=CARTESIAN_POINT('Ctrl Pts',(1.24558623976355,-0.990330805779366,
1.90869858745619));
#22091=CARTESIAN_POINT('Ctrl Pts',(1.28099787676127,-1.02450444247951,1.85971261136954));
#22092=CARTESIAN_POINT('Ctrl Pts',(1.31864023203821,-1.04239377091596,1.81924683990037));
#22093=CARTESIAN_POINT('Ctrl Pts',(1.41407631065895,-1.06560081915269,1.72946791921561));
#22094=CARTESIAN_POINT('Ctrl Pts',(1.46561476759698,-1.07189861347413,1.68453186313418));
#22095=CARTESIAN_POINT('Ctrl Pts',(1.52399042602929,-1.07301833748062,1.63615580822897));
#22096=CARTESIAN_POINT('',(1.59279130921887,-0.967951970128402,1.63615580822897));
#22097=CARTESIAN_POINT('Origin',(0.,0.,1.63615580822897));
#22098=CARTESIAN_POINT('',(1.41284463836769,-0.732195474855993,1.90869858745619));
#22099=CARTESIAN_POINT('Ctrl Pts',(1.59279130921887,-0.967951970128402,
1.63615580822897));
#22100=CARTESIAN_POINT('Ctrl Pts',(1.58042744248116,-0.93071971304077,1.66605750083532));
#22101=CARTESIAN_POINT('Ctrl Pts',(1.56278639305871,-0.887832231474075,
1.7027884126318));
#22102=CARTESIAN_POINT('Ctrl Pts',(1.52428552078368,-0.824582081178599,
1.76702045133218));
#22103=CARTESIAN_POINT('Ctrl Pts',(1.50612290809471,-0.798317781239404,
1.79540516147646));
#22104=CARTESIAN_POINT('Ctrl Pts',(1.46790189965391,-0.761468116018828,
1.84635863460502));
#22105=CARTESIAN_POINT('Ctrl Pts',(1.44591574321668,-0.744952250887404,
1.87346655258662));
#22106=CARTESIAN_POINT('Ctrl Pts',(1.41284463836769,-0.732195474855994,
1.90869858745619));
#22107=CARTESIAN_POINT('',(1.49065195897357,-0.556953250077771,1.90869858745619));
#22108=CARTESIAN_POINT('Ctrl Pts',(1.41284463836769,-0.732195474855994,
1.90869858745619));
#22109=CARTESIAN_POINT('Ctrl Pts',(1.42701478571971,-0.702714598502428,
1.90968240330487));
#22110=CARTESIAN_POINT('Ctrl Pts',(1.44068509220622,-0.673005678918828,
1.91020759224355));
#22111=CARTESIAN_POINT('Ctrl Pts',(1.45391861530618,-0.643086573508103,
1.91020766105751));
#22112=CARTESIAN_POINT('Ctrl Pts',(1.46655152316666,-0.614525373360053,
1.91020772674828));
#22113=CARTESIAN_POINT('Ctrl Pts',(1.47877245207676,-0.585803416586618,
1.90972920064616));
#22114=CARTESIAN_POINT('Ctrl Pts',(1.49065195897357,-0.556953250077771,
1.90869858745619));
#22115=CARTESIAN_POINT('',(1.78098192700405,-0.54956214105737,1.63615580822897));
#22116=CARTESIAN_POINT('Ctrl Pts',(1.49065195897357,-0.556953250077771,
1.90869858745619));
#22117=CARTESIAN_POINT('Ctrl Pts',(1.53489066158786,-0.578511512313559,
1.85971261137509));
#22118=CARTESIAN_POINT('Ctrl Pts',(1.57621877536647,-0.583893147209275,
1.8192468399059));
#22119=CARTESIAN_POINT('Ctrl Pts',(1.67415525211499,-0.576472991488994,
1.72946791922834));
#22120=CARTESIAN_POINT('Ctrl Pts',(1.72511736289743,-0.56653629076237,1.68453186314677));
#22121=CARTESIAN_POINT('Ctrl Pts',(1.78098192700405,-0.549562141057369,
1.63615580822897));
#22122=CARTESIAN_POINT('Origin',(0.,0.,1.63615580822897));
#22123=CARTESIAN_POINT('',(1.85754313061971,0.153129647965885,1.63615580822897));
#22124=CARTESIAN_POINT('Origin',(0.,0.,1.63615580822897));
#22125=CARTESIAN_POINT('',(1.57338902476662,0.238090659850088,1.90869858745619));
#22126=CARTESIAN_POINT('Ctrl Pts',(1.85754313061971,0.153129647965885,1.63615580822897));
#22127=CARTESIAN_POINT('Ctrl Pts',(1.82091613387028,0.179381031885754,1.670502220505));
#22128=CARTESIAN_POINT('Ctrl Pts',(1.7769385116542,0.205636042642618,1.71137352645763));
#22129=CARTESIAN_POINT('Ctrl Pts',(1.68891823997117,0.239331856619953,1.79432582270636));
#22130=CARTESIAN_POINT('Ctrl Pts',(1.66303434064729,0.243146486728477,1.81928768858642));
#22131=CARTESIAN_POINT('Ctrl Pts',(1.6309352979637,0.246645694090263,1.85052786620714));
#22132=CARTESIAN_POINT('Ctrl Pts',(1.60542169144917,0.24661777674522,1.87575066654868));
#22133=CARTESIAN_POINT('Ctrl Pts',(1.57338902476662,0.238090659850087,1.90869858745619));
#22134=CARTESIAN_POINT('',(1.53333167412,0.425598593400271,1.90869858745619));
#22135=CARTESIAN_POINT('Ctrl Pts',(1.57338902476662,0.238090659850087,1.90869858745619));
#22136=CARTESIAN_POINT('Ctrl Pts',(1.56752449044192,0.270270193465537,1.90968240330487));
#22137=CARTESIAN_POINT('Ctrl Pts',(1.56112153591504,0.30234041884027,1.91020759224355));
#22138=CARTESIAN_POINT('Ctrl Pts',(1.55424167207615,0.334323953288058,1.91020766105751));
#22139=CARTESIAN_POINT('Ctrl Pts',(1.54767405698885,0.36485588652155,1.91020772674828));
#22140=CARTESIAN_POINT('Ctrl Pts',(1.54067865355577,0.395275719445624,1.90972920064616));
#22141=CARTESIAN_POINT('Ctrl Pts',(1.53333167412,0.425598593400271,1.90869858745619));
#22142=CARTESIAN_POINT('',(1.76386916735272,0.602229799711917,1.63615580822897));
#22143=CARTESIAN_POINT('Ctrl Pts',(1.53333167412,0.425598593400271,1.90869858745619));
#22144=CARTESIAN_POINT('Ctrl Pts',(1.58179316495472,0.434160449860156,1.85971261137164));
#22145=CARTESIAN_POINT('Ctrl Pts',(1.61839155697147,0.454098671557975,1.81924683990245));
#22146=CARTESIAN_POINT('Ctrl Pts',(1.69326237294042,0.517667320341299,1.72946791921015));
#22147=CARTESIAN_POINT('Ctrl Pts',(1.72865094048853,0.555661057247196,1.6845318631267));
#22148=CARTESIAN_POINT('Ctrl Pts',(1.76386916735272,0.602229799711918,1.63615580822897));
#22149=CARTESIAN_POINT('',(1.71930883511106,0.71964734468187,1.63615580822897));
#22150=CARTESIAN_POINT('Origin',(0.,0.,1.63615580822897));
#22151=CARTESIAN_POINT('',(1.42280782457595,0.712641620935351,1.90869858745619));
#22152=CARTESIAN_POINT('Ctrl Pts',(1.71930883511106,0.71964734468187,1.63615580822897));
#22153=CARTESIAN_POINT('Ctrl Pts',(1.68192000785468,0.731529338001752,1.66605750083837));
#22154=CARTESIAN_POINT('Ctrl Pts',(1.63685415773697,0.742466058392258,1.7027884126341));
#22155=CARTESIAN_POINT('Ctrl Pts',(1.56305346633102,0.748495703972178,1.76702045133142));
#22156=CARTESIAN_POINT('Ctrl Pts',(1.53112948545266,0.749239609810725,1.79540516147611));
#22157=CARTESIAN_POINT('Ctrl Pts',(1.47885173496202,0.739977854208386,1.84635863460557));
#22158=CARTESIAN_POINT('Ctrl Pts',(1.45256698088552,0.731898461962535,1.87346655258725));
#22159=CARTESIAN_POINT('Ctrl Pts',(1.42280782457595,0.71264162093535,1.90869858745619));
#22160=CARTESIAN_POINT('',(1.32676788217082,0.878593860895846,1.90869858745619));
#22161=CARTESIAN_POINT('Ctrl Pts',(1.42280782457595,0.71264162093535,1.90869858745619));
#22162=CARTESIAN_POINT('Ctrl Pts',(1.40728629823316,0.741433935301243,1.90968240330488));
#22163=CARTESIAN_POINT('Ctrl Pts',(1.39128648195261,0.769955910359918,1.91020759224355));
#22164=CARTESIAN_POINT('Ctrl Pts',(1.37485988693288,0.798248064365429,1.91020766105751));
#22165=CARTESIAN_POINT('Ctrl Pts',(1.35917882756731,0.825256153747737,1.91020772674828));
#22166=CARTESIAN_POINT('Ctrl Pts',(1.34312555820857,0.852025435531456,1.90972920064616));
#22167=CARTESIAN_POINT('Ctrl Pts',(1.32676788217082,0.878593860895846,1.90869858745619));
#22168=CARTESIAN_POINT('',(1.4914400228729,1.11782012388912,1.63615580822897));
#22169=CARTESIAN_POINT('Ctrl Pts',(1.32676788217082,0.878593860895847,1.90869858745619));
#22170=CARTESIAN_POINT('Ctrl Pts',(1.37021173966576,0.901712094512517,1.85971261137537));
#22171=CARTESIAN_POINT('Ctrl Pts',(1.39885762953817,0.93198399527982,1.81924683990615));
#22172=CARTESIAN_POINT('Ctrl Pts',(1.45042021415007,1.01557772743474,1.72946791923503));
#22173=CARTESIAN_POINT('Ctrl Pts',(1.4723360315385,1.06264758726748,1.68453186315486));
#22174=CARTESIAN_POINT('Ctrl Pts',(1.4914400228729,1.11782012388912,1.63615580822897));
#22175=CARTESIAN_POINT('',(1.4127766116927,1.21572094522251,1.63615580822897));
#22176=CARTESIAN_POINT('Origin',(0.,0.,1.63615580822897));
#22177=CARTESIAN_POINT('',(1.13295228123076,1.11743425489732,1.90869858745619));
#22178=CARTESIAN_POINT('Ctrl Pts',(1.4127766116927,1.21572094522251,1.63615580822897));
#22179=CARTESIAN_POINT('Ctrl Pts',(1.37354598600622,1.21546760937383,1.66605750085724));
#22180=CARTESIAN_POINT('Ctrl Pts',(1.3273061831347,1.21194293501213,1.70278841264844));
#22181=CARTESIAN_POINT('Ctrl Pts',(1.2552542917288,1.19487180089487,1.76702045133053));
#22182=CARTESIAN_POINT('Ctrl Pts',(1.22466290214095,1.18571424477033,1.79540516147619));
#22183=CARTESIAN_POINT('Ctrl Pts',(1.17780584675802,1.16075107842286,1.84635863460612));
#22184=CARTESIAN_POINT('Ctrl Pts',(1.15530422962257,1.14494468407682,1.873466552588));
#22185=CARTESIAN_POINT('Ctrl Pts',(1.13295228123076,1.11743425489733,1.90869858745619));
#22186=CARTESIAN_POINT('',(0.990330805779366,1.24558623976355,1.90869858745619));
#22187=CARTESIAN_POINT('Ctrl Pts',(1.13295228123076,1.11743425489732,1.90869858745619));
#22188=CARTESIAN_POINT('Ctrl Pts',(1.10929311801315,1.14002095767567,1.90968240330487));
#22189=CARTESIAN_POINT('Ctrl Pts',(1.08526261347374,1.16220275277526,1.91020759224355));
#22190=CARTESIAN_POINT('Ctrl Pts',(1.0608972368445,1.18403409318141,1.91020766105751));
#22191=CARTESIAN_POINT('Ctrl Pts',(1.03763770454776,1.20487459874736,1.91020772674828));
#22192=CARTESIAN_POINT('Ctrl Pts',(1.0140979751179,1.22537296557719,1.90972920064616));
#22193=CARTESIAN_POINT('Ctrl Pts',(0.990330805779366,1.24558623976355,1.90869858745619));
#22194=CARTESIAN_POINT('',(1.07301833748062,1.52399042602929,1.63615580822897));
#22195=CARTESIAN_POINT('Ctrl Pts',(0.990330805779366,1.24558623976356,1.90869858745619));
#22196=CARTESIAN_POINT('Ctrl Pts',(1.02450444247754,1.28099787675924,1.85971261137236));
#22197=CARTESIAN_POINT('Ctrl Pts',(1.04239377091547,1.31864023203516,1.81924683990311));
#22198=CARTESIAN_POINT('Ctrl Pts',(1.06560081915497,1.41407631066917,1.72946791920612));
#22199=CARTESIAN_POINT('Ctrl Pts',(1.07189861347441,1.46561476761072,1.68453186312278));
#22200=CARTESIAN_POINT('Ctrl Pts',(1.07301833748062,1.52399042602929,1.63615580822897));
#22201=CARTESIAN_POINT('',(0.967951970128401,1.59279130921887,1.63615580822897));
#22202=CARTESIAN_POINT('Origin',(0.,0.,1.63615580822897));
#22203=CARTESIAN_POINT('',(0.732195474855993,1.41284463836769,1.90869858745619));
#22204=CARTESIAN_POINT('Ctrl Pts',(0.967951970128401,1.59279130921887,1.63615580822897));
#22205=CARTESIAN_POINT('Ctrl Pts',(0.930719713031906,1.58042744247821,1.66605750084244));
#22206=CARTESIAN_POINT('Ctrl Pts',(0.887832231468784,1.56278639305548,1.70278841263718));
#22207=CARTESIAN_POINT('Ctrl Pts',(0.824582081181466,1.52428552078543,1.76702045132927));
#22208=CARTESIAN_POINT('Ctrl Pts',(0.798317781240507,1.50612290809584,1.79540516147495));
#22209=CARTESIAN_POINT('Ctrl Pts',(0.761468116016308,1.46790189965131,1.84635863460849));
#22210=CARTESIAN_POINT('Ctrl Pts',(0.744952250886103,1.44591574321331,1.87346655259021));
#22211=CARTESIAN_POINT('Ctrl Pts',(0.732195474855993,1.41284463836769,1.90869858745619));
#22212=CARTESIAN_POINT('',(0.55695325007777,1.49065195897357,1.90869858745619));
#22213=CARTESIAN_POINT('Ctrl Pts',(0.732195474855993,1.41284463836769,1.90869858745619));
#22214=CARTESIAN_POINT('Ctrl Pts',(0.702714598502391,1.42701478571972,1.90968240330487));
#22215=CARTESIAN_POINT('Ctrl Pts',(0.67300567891881,1.44068509220623,1.91020759224355));
#22216=CARTESIAN_POINT('Ctrl Pts',(0.643086573508102,1.45391861530618,1.91020766105751));
#22217=CARTESIAN_POINT('Ctrl Pts',(0.614525373360064,1.46655152316665,1.91020772674828));
#22218=CARTESIAN_POINT('Ctrl Pts',(0.585803416586623,1.47877245207676,1.90972920064616));
#22219=CARTESIAN_POINT('Ctrl Pts',(0.55695325007777,1.49065195897357,1.90869858745619));
#22220=CARTESIAN_POINT('',(0.549562141057369,1.78098192700405,1.63615580822897));
#22221=CARTESIAN_POINT('Ctrl Pts',(0.55695325007777,1.49065195897357,1.90869858745619));
#22222=CARTESIAN_POINT('Ctrl Pts',(0.578511512313229,1.53489066158716,1.85971261137586));
#22223=CARTESIAN_POINT('Ctrl Pts',(0.583893147209425,1.57621877536565,1.81924683990662));
#22224=CARTESIAN_POINT('Ctrl Pts',(0.57647299149051,1.67415525209398,1.72946791924761));
#22225=CARTESIAN_POINT('Ctrl Pts',(0.566536290770542,1.72511736287052,1.68453186317007));
#22226=CARTESIAN_POINT('Ctrl Pts',(0.549562141057369,1.78098192700405,1.63615580822897));
#22227=CARTESIAN_POINT('',(0.428377445609994,1.81394816223928,1.63615580822897));
#22228=CARTESIAN_POINT('Origin',(0.,0.,1.63615580822897));
#22229=CARTESIAN_POINT('',(0.259766273896474,1.5699559447672,1.90869858745619));
#22230=CARTESIAN_POINT('Ctrl Pts',(0.428377445609995,1.81394816223928,1.63615580822897));
#22231=CARTESIAN_POINT('Ctrl Pts',(0.396788109845208,1.79068402604501,1.66605750081957));
#22232=CARTESIAN_POINT('Ctrl Pts',(0.361451075096166,1.76065343038563,1.70278841261988));
#22233=CARTESIAN_POINT('Ctrl Pts',(0.313194031326,1.70449155358005,1.7670204513286));
#22234=CARTESIAN_POINT('Ctrl Pts',(0.29382775370454,1.67910176740199,1.79540516147386));
#22235=CARTESIAN_POINT('Ctrl Pts',(0.270592580620559,1.63136425546867,1.84635863460898));
#22236=CARTESIAN_POINT('Ctrl Pts',(0.261679155446751,1.60535049511798,1.87346655259067));
#22237=CARTESIAN_POINT('Ctrl Pts',(0.259766273896474,1.5699559447672,1.90869858745619));
#22238=CARTESIAN_POINT('',(0.0690572297370888,1.58980227845634,1.90869858745619));
#22239=CARTESIAN_POINT('Ctrl Pts',(0.259766273896474,1.5699559447672,1.90869858745619));
#22240=CARTESIAN_POINT('Ctrl Pts',(0.227349477989723,1.57432246394088,1.90968240330487));
#22241=CARTESIAN_POINT('Ctrl Pts',(0.194870259405019,1.57814313696878,1.91020759224355));
#22242=CARTESIAN_POINT('Ctrl Pts',(0.162326115709102,1.58148345331813,1.91020766105751));
#22243=CARTESIAN_POINT('Ctrl Pts',(0.131259016977809,1.5846721664331,1.91020772674828));
#22244=CARTESIAN_POINT('Ctrl Pts',(0.100166338107427,1.58741938775354,1.90972920064616));
#22245=CARTESIAN_POINT('Ctrl Pts',(0.0690572297370895,1.58980227845634,
1.90869858745619));
#22246=CARTESIAN_POINT('',(-0.0276890267571665,1.86363850813291,1.63615580822897));
#22247=CARTESIAN_POINT('Ctrl Pts',(0.0690572297370894,1.58980227845634,
1.90869858745619));
#22248=CARTESIAN_POINT('Ctrl Pts',(0.0758898445998494,1.63853765425239,
1.85971261137284));
#22249=CARTESIAN_POINT('Ctrl Pts',(0.0682369940313255,1.67950604280803,
1.81924683990368));
#22250=CARTESIAN_POINT('Ctrl Pts',(0.0309159708965805,1.77035621298606,
1.72946791922431));
#22251=CARTESIAN_POINT('Ctrl Pts',(0.00571744861764431,1.81575345113751,
1.68453186314245));
#22252=CARTESIAN_POINT('Ctrl Pts',(-0.0276890267571666,1.86363850813291,
1.63615580822897));
#22253=CARTESIAN_POINT('',(-0.153129647965885,1.85754313061971,1.63615580822897));
#22254=CARTESIAN_POINT('Origin',(0.,0.,1.63615580822897));
#22255=CARTESIAN_POINT('',(-0.238090659850087,1.57338902476662,1.90869858745619));
#22256=CARTESIAN_POINT('Ctrl Pts',(-0.153129647965885,1.85754313061971,
1.63615580822897));
#22257=CARTESIAN_POINT('Ctrl Pts',(-0.179418518274793,1.8208638313382,1.67055126641347));
#22258=CARTESIAN_POINT('Ctrl Pts',(-0.20567438065217,1.77686224466177,1.71144473813517));
#22259=CARTESIAN_POINT('Ctrl Pts',(-0.239335933326219,1.6888882678776,1.79435460643136));
#22260=CARTESIAN_POINT('Ctrl Pts',(-0.243149658729012,1.66302384256867,
1.8192976251428));
#22261=CARTESIAN_POINT('Ctrl Pts',(-0.246644834768781,1.63091267750131,
1.8505503416528));
#22262=CARTESIAN_POINT('Ctrl Pts',(-0.246614602123229,1.60540976577613,
1.87576293296834));
#22263=CARTESIAN_POINT('Ctrl Pts',(-0.238090659850087,1.57338902476663,
1.90869858745619));
#22264=CARTESIAN_POINT('',(-0.425598593400271,1.53333167412,1.90869858745619));
#22265=CARTESIAN_POINT('Ctrl Pts',(-0.238090659850087,1.57338902476662,
1.90869858745619));
#22266=CARTESIAN_POINT('Ctrl Pts',(-0.270270193465531,1.56752449044192,
1.90968240330487));
#22267=CARTESIAN_POINT('Ctrl Pts',(-0.302340418840268,1.56112153591504,
1.91020759224355));
#22268=CARTESIAN_POINT('Ctrl Pts',(-0.334323953288058,1.55424167207615,
1.91020766105751));
#22269=CARTESIAN_POINT('Ctrl Pts',(-0.364855886521545,1.54767405698885,
1.91020772674828));
#22270=CARTESIAN_POINT('Ctrl Pts',(-0.395275719445621,1.54067865355577,
1.90972920064616));
#22271=CARTESIAN_POINT('Ctrl Pts',(-0.425598593400271,1.53333167412,1.90869858745619));
#22272=CARTESIAN_POINT('',(-0.602229799711917,1.76386916735272,1.63615580822897));
#22273=CARTESIAN_POINT('Ctrl Pts',(-0.425598593400271,1.53333167412,1.90869858745619));
#22274=CARTESIAN_POINT('Ctrl Pts',(-0.434160449860446,1.58179316495636,
1.85971261136998));
#22275=CARTESIAN_POINT('Ctrl Pts',(-0.454098671559147,1.61839155697284,
1.8192468399008));
#22276=CARTESIAN_POINT('Ctrl Pts',(-0.517667320349084,1.6932623729496,1.72946791919914));
#22277=CARTESIAN_POINT('Ctrl Pts',(-0.555661057259041,1.72865094049748,
1.6845318631144));
#22278=CARTESIAN_POINT('Ctrl Pts',(-0.602229799711917,1.76386916735272,
1.63615580822897));
#22279=CARTESIAN_POINT('',(-0.71964734468187,1.71930883511106,1.63615580822897));
#22280=CARTESIAN_POINT('Origin',(0.,0.,1.63615580822897));
#22281=CARTESIAN_POINT('',(-0.712641620935351,1.42280782457595,1.90869858745619));
#22282=CARTESIAN_POINT('Ctrl Pts',(-0.71964734468187,1.71930883511106,1.63615580822897));
#22283=CARTESIAN_POINT('Ctrl Pts',(-0.731529338009184,1.6819200078313,1.66605750085707));
#22284=CARTESIAN_POINT('Ctrl Pts',(-0.742466058393576,1.63685415772068,
1.70278841264829));
#22285=CARTESIAN_POINT('Ctrl Pts',(-0.748495703972309,1.56305346632953,
1.76702045133272));
#22286=CARTESIAN_POINT('Ctrl Pts',(-0.749239609810482,1.53112948545126,
1.79540516147747));
#22287=CARTESIAN_POINT('Ctrl Pts',(-0.739977854208578,1.47885173496312,
1.8463586346045));
#22288=CARTESIAN_POINT('Ctrl Pts',(-0.731898461963124,1.45256698088643,
1.87346655258617));
#22289=CARTESIAN_POINT('Ctrl Pts',(-0.71264162093535,1.42280782457595,1.90869858745619));
#22290=CARTESIAN_POINT('',(-0.878593860895847,1.32676788217082,1.90869858745619));
#22291=CARTESIAN_POINT('Ctrl Pts',(-0.712641620935351,1.42280782457595,
1.90869858745619));
#22292=CARTESIAN_POINT('Ctrl Pts',(-0.741433935301275,1.40728629823315,
1.90968240330488));
#22293=CARTESIAN_POINT('Ctrl Pts',(-0.769955910359934,1.3912864819526,1.91020759224355));
#22294=CARTESIAN_POINT('Ctrl Pts',(-0.798248064365429,1.37485988693287,
1.91020766105751));
#22295=CARTESIAN_POINT('Ctrl Pts',(-0.82525615374773,1.35917882756732,1.91020772674828));
#22296=CARTESIAN_POINT('Ctrl Pts',(-0.852025435531453,1.34312555820858,
1.90972920064616));
#22297=CARTESIAN_POINT('Ctrl Pts',(-0.878593860895846,1.32676788217082,
1.90869858745619));
#22298=CARTESIAN_POINT('',(-1.11782012388912,1.4914400228729,1.63615580822897));
#22299=CARTESIAN_POINT('Ctrl Pts',(-0.878593860895847,1.32676788217082,
1.90869858745619));
#22300=CARTESIAN_POINT('Ctrl Pts',(-0.901712094513524,1.37021173966765,
1.85971261137323));
#22301=CARTESIAN_POINT('Ctrl Pts',(-0.931983995281799,1.39885762953939,
1.81924683990403));
#22302=CARTESIAN_POINT('Ctrl Pts',(-1.01557772743753,1.45042021415179,1.72946791923204));
#22303=CARTESIAN_POINT('Ctrl Pts',(-1.06264758727016,1.47233603153943,1.68453186315251));
#22304=CARTESIAN_POINT('Ctrl Pts',(-1.11782012388912,1.4914400228729,1.63615580822897));
#22305=CARTESIAN_POINT('',(-1.21572094522251,1.4127766116927,1.63615580822897));
#22306=CARTESIAN_POINT('Origin',(0.,0.,1.63615580822897));
#22307=CARTESIAN_POINT('',(-1.11743425489732,1.13295228123076,1.90869858745619));
#22308=CARTESIAN_POINT('Ctrl Pts',(-1.21572094522251,1.4127766116927,1.63615580822897));
#22309=CARTESIAN_POINT('Ctrl Pts',(-1.21546760937391,1.37354598601819,1.66605750084812));
#22310=CARTESIAN_POINT('Ctrl Pts',(-1.21194293501399,1.32730618314253,1.70278841264146));
#22311=CARTESIAN_POINT('Ctrl Pts',(-1.19487180089464,1.25525429172787,1.76702045133136));
#22312=CARTESIAN_POINT('Ctrl Pts',(-1.18571424477025,1.2246629021408,1.79540516147636));
#22313=CARTESIAN_POINT('Ctrl Pts',(-1.16075107842331,1.17780584675887,1.84635863460519));
#22314=CARTESIAN_POINT('Ctrl Pts',(-1.14494468407762,1.15530422962322,1.87346655258698));
#22315=CARTESIAN_POINT('Ctrl Pts',(-1.11743425489732,1.13295228123076,1.90869858745619));
#22316=CARTESIAN_POINT('',(-1.24558623976355,0.990330805779366,1.90869858745619));
#22317=CARTESIAN_POINT('Ctrl Pts',(-1.11743425489732,1.13295228123076,1.90869858745619));
#22318=CARTESIAN_POINT('Ctrl Pts',(-1.14002095767565,1.10929311801317,1.90968240330487));
#22319=CARTESIAN_POINT('Ctrl Pts',(-1.16220275277525,1.08526261347375,1.91020759224355));
#22320=CARTESIAN_POINT('Ctrl Pts',(-1.18403409318141,1.0608972368445,1.91020766105751));
#22321=CARTESIAN_POINT('Ctrl Pts',(-1.20487459874736,1.03763770454776,1.91020772674828));
#22322=CARTESIAN_POINT('Ctrl Pts',(-1.22537296557719,1.0140979751179,1.90972920064616));
#22323=CARTESIAN_POINT('Ctrl Pts',(-1.24558623976355,0.990330805779366,
1.90869858745619));
#22324=CARTESIAN_POINT('',(-1.52399042602929,1.07301833748062,1.63615580822897));
#22325=CARTESIAN_POINT('Ctrl Pts',(-1.24558623976355,0.990330805779367,
1.90869858745619));
#22326=CARTESIAN_POINT('Ctrl Pts',(-1.28099787675963,1.02450444247792,1.85971261137182));
#22327=CARTESIAN_POINT('Ctrl Pts',(-1.31864023203577,1.04239377091547,1.81924683990261));
#22328=CARTESIAN_POINT('Ctrl Pts',(-1.41407631064749,1.06560081914982,1.72946791922645));
#22329=CARTESIAN_POINT('Ctrl Pts',(-1.46561476758198,1.07189861347385,1.68453186314661));
#22330=CARTESIAN_POINT('Ctrl Pts',(-1.52399042602929,1.07301833748062,1.63615580822897));
#22331=CARTESIAN_POINT('',(-1.59279130921887,0.967951970128402,1.63615580822897));
#22332=CARTESIAN_POINT('Origin',(0.,0.,1.63615580822897));
#22333=CARTESIAN_POINT('',(-1.41284463836769,0.732195474855993,1.90869858745619));
#22334=CARTESIAN_POINT('Ctrl Pts',(-1.59279130921887,0.967951970128402,
1.63615580822897));
#22335=CARTESIAN_POINT('Ctrl Pts',(-1.58042744247569,0.930719713024315,
1.66605750084853));
#22336=CARTESIAN_POINT('Ctrl Pts',(-1.56278639305271,0.887832231464228,
1.70278841264181));
#22337=CARTESIAN_POINT('Ctrl Pts',(-1.52428552078413,0.824582081179332,
1.76702045133144));
#22338=CARTESIAN_POINT('Ctrl Pts',(-1.50612290809471,0.798317781239413,
1.79540516147645));
#22339=CARTESIAN_POINT('Ctrl Pts',(-1.46790189965197,0.761468116016952,
1.84635863460761));
#22340=CARTESIAN_POINT('Ctrl Pts',(-1.44591574321434,0.744952250886503,
1.87346655258912));
#22341=CARTESIAN_POINT('Ctrl Pts',(-1.41284463836769,0.732195474855993,
1.90869858745619));
#22342=CARTESIAN_POINT('',(-1.49065195897357,0.55695325007777,1.90869858745619));
#22343=CARTESIAN_POINT('Ctrl Pts',(-1.41284463836769,0.732195474855993,
1.90869858745619));
#22344=CARTESIAN_POINT('Ctrl Pts',(-1.42701478571972,0.70271459850241,1.90968240330487));
#22345=CARTESIAN_POINT('Ctrl Pts',(-1.44068509220623,0.673005678918819,
1.91020759224355));
#22346=CARTESIAN_POINT('Ctrl Pts',(-1.45391861530618,0.643086573508102,
1.91020766105751));
#22347=CARTESIAN_POINT('Ctrl Pts',(-1.46655152316666,0.614525373360044,
1.91020772674828));
#22348=CARTESIAN_POINT('Ctrl Pts',(-1.47877245207676,0.585803416586613,
1.90972920064616));
#22349=CARTESIAN_POINT('Ctrl Pts',(-1.49065195897357,0.55695325007777,1.90869858745619));
#22350=CARTESIAN_POINT('',(-1.78098192700405,0.549562141057368,1.63615580822897));
#22351=CARTESIAN_POINT('Ctrl Pts',(-1.49065195897357,0.55695325007777,1.90869858745619));
#22352=CARTESIAN_POINT('Ctrl Pts',(-1.53489066159152,0.578511512315346,
1.85971261137103));
#22353=CARTESIAN_POINT('Ctrl Pts',(-1.57621877537088,0.583893147208912,
1.81924683990186));
#22354=CARTESIAN_POINT('Ctrl Pts',(-1.67415525213672,0.576472991487369,
1.7294679192084));
#22355=CARTESIAN_POINT('Ctrl Pts',(-1.72511736292283,0.566536290754648,
1.68453186312477));
#22356=CARTESIAN_POINT('Ctrl Pts',(-1.78098192700405,0.549562141057369,
1.63615580822897));
#22357=CARTESIAN_POINT('',(-1.81394816223928,0.428377445609995,1.63615580822897));
#22358=CARTESIAN_POINT('Origin',(0.,0.,1.63615580822897));
#22359=CARTESIAN_POINT('',(-1.5699559447672,0.259766273896474,1.90869858745619));
#22360=CARTESIAN_POINT('Ctrl Pts',(-1.81394816223928,0.428377445609995,
1.63615580822897));
#22361=CARTESIAN_POINT('Ctrl Pts',(-1.79068402603114,0.396788109826372,
1.6660575008374));
#22362=CARTESIAN_POINT('Ctrl Pts',(-1.76065343037378,0.361451075086,1.70278841263343));
#22363=CARTESIAN_POINT('Ctrl Pts',(-1.70449155357908,0.313194031325156,
1.76702045132971));
#22364=CARTESIAN_POINT('Ctrl Pts',(-1.67910176740082,0.293827753703966,
1.79540516147511));
#22365=CARTESIAN_POINT('Ctrl Pts',(-1.6313642554699,0.270592580621158,1.84635863460767));
#22366=CARTESIAN_POINT('Ctrl Pts',(-1.60535049511926,0.261679155446819,
1.8734665525894));
#22367=CARTESIAN_POINT('Ctrl Pts',(-1.5699559447672,0.259766273896474,1.90869858745619));
#22368=CARTESIAN_POINT('',(-1.58980227845634,0.0690572297370887,1.90869858745619));
#22369=CARTESIAN_POINT('Ctrl Pts',(-1.5699559447672,0.259766273896474,1.90869858745619));
#22370=CARTESIAN_POINT('Ctrl Pts',(-1.57432246394088,0.227349477989734,
1.90968240330487));
#22371=CARTESIAN_POINT('Ctrl Pts',(-1.57814313696878,0.194870259405024,
1.91020759224355));
#22372=CARTESIAN_POINT('Ctrl Pts',(-1.58148345331813,0.162326115709102,
1.91020766105751));
#22373=CARTESIAN_POINT('Ctrl Pts',(-1.5846721664331,0.131259016977824,1.91020772674828));
#22374=CARTESIAN_POINT('Ctrl Pts',(-1.58741938775354,0.100166338107434,
1.90972920064616));
#22375=CARTESIAN_POINT('Ctrl Pts',(-1.58980227845634,0.0690572297370887,
1.90869858745619));
#22376=CARTESIAN_POINT('Ctrl Pts',(-1.58980227845634,0.0690572297370892,
1.90869858745619));
#22377=CARTESIAN_POINT('Ctrl Pts',(-1.63853765425085,0.0758898445996293,
1.85971261137438));
#22378=CARTESIAN_POINT('Ctrl Pts',(-1.67950604280655,0.0682369940321497,
1.81924683990515));
#22379=CARTESIAN_POINT('Ctrl Pts',(-1.75795323731548,0.0360110823424086,
1.7417246466111));
#22380=CARTESIAN_POINT('Ctrl Pts',(-1.78904228717242,0.0200459877611124,
1.71095771283311));
#22381=CARTESIAN_POINT('Ctrl Pts',(-1.82153560297087,-5.02124314349928E-10,
1.67846439702913));
#22382=CARTESIAN_POINT('Origin',(0.,0.,1.37171309575435));
#22383=CARTESIAN_POINT('',(1.23077165948193,-0.27609248605186,1.10727038327973));
#22384=CARTESIAN_POINT('Origin',(0.,0.,1.10727038327973));
#22385=CARTESIAN_POINT('Ctrl Pts',(1.23077165948193,-0.27609248605186,1.10727038327973));
#22386=CARTESIAN_POINT('Ctrl Pts',(1.31709676330276,-0.275172898999399,
1.1810356590104));
#22387=CARTESIAN_POINT('Ctrl Pts',(1.40429909999041,-0.260135222790519,
1.25302429310882));
#22388=CARTESIAN_POINT('Ctrl Pts',(1.57126422405226,-0.18954862836963,1.38870233571737));
#22389=CARTESIAN_POINT('Ctrl Pts',(1.64663281162092,-0.136344571823203,
1.44896010631748));
#22390=CARTESIAN_POINT('Ctrl Pts',(1.77081457368154,-0.00172234028007623,
1.55344588116294));
#22391=CARTESIAN_POINT('Ctrl Pts',(1.81885265993609,0.0722540415540171,
1.5964737415496));
#22392=CARTESIAN_POINT('Ctrl Pts',(1.85754313061971,0.153129647965885,1.63615580822897));
#22393=CARTESIAN_POINT('Origin',(0.,0.,1.37171309575435));
#22394=CARTESIAN_POINT('',(1.03556549162895,-0.720159740047642,1.10727038327973));
#22395=CARTESIAN_POINT('Ctrl Pts',(1.78098192700405,-0.54956214105737,1.63615580822897));
#22396=CARTESIAN_POINT('Ctrl Pts',(1.70079633666899,-0.620893161259095,
1.58735805514614));
#22397=CARTESIAN_POINT('Ctrl Pts',(1.61925404078172,-0.674133367258213,
1.53858095020842));
#22398=CARTESIAN_POINT('Ctrl Pts',(1.4446131950236,-0.751969574388251,1.42806953503214));
#22399=CARTESIAN_POINT('Ctrl Pts',(1.3500715267369,-0.772017157909611,1.36461306044572));
#22400=CARTESIAN_POINT('Ctrl Pts',(1.1777963531315,-0.767479006699501,1.23357020765532));
#22401=CARTESIAN_POINT('Ctrl Pts',(1.10397180136272,-0.749676646324455,
1.17136442658356));
#22402=CARTESIAN_POINT('Ctrl Pts',(1.03556549162895,-0.720159740047643,
1.10727038327973));
#22403=CARTESIAN_POINT('Origin',(0.,0.,1.10727038327973));
#22404=CARTESIAN_POINT('Ctrl Pts',(0.759649337735664,-0.764532229233201,
1.28318567027397));
#22405=CARTESIAN_POINT('Ctrl Pts',(0.951374367053297,-0.889432488376419,
1.53751096017972));
#22406=CARTESIAN_POINT('Ctrl Pts',(1.16919064445972,-0.87860280381325,1.74607168007008));
#22407=CARTESIAN_POINT('Ctrl Pts',(1.41309816995492,-0.732043175543693,
1.90886782994506));
#22408=CARTESIAN_POINT('Ctrl Pts',(0.771069504093749,-0.773880285955837,
1.26847940010162));
#22409=CARTESIAN_POINT('Ctrl Pts',(0.965585896981729,-0.900241293626995,
1.51987665322459));
#22410=CARTESIAN_POINT('Ctrl Pts',(1.18626243797172,-0.888897245689574,
1.72611612827485));
#22411=CARTESIAN_POINT('Ctrl Pts',(1.43333134754251,-0.739998335618526,
1.88704325648017));
#22412=CARTESIAN_POINT('Ctrl Pts',(0.79001938035927,-0.793756470105421,
1.24117952306876));
#22413=CARTESIAN_POINT('Ctrl Pts',(0.989358920654672,-0.923380672132911,
1.48716712955728));
#22414=CARTESIAN_POINT('Ctrl Pts',(1.21569285383182,-0.911936310735738,
1.68888851879238));
#22415=CARTESIAN_POINT('Ctrl Pts',(1.46902007592141,-0.759433295933255,
1.84634532147278));
#22416=CARTESIAN_POINT('Ctrl Pts',(0.818798433422952,-0.852549487780081,
1.18072779772815));
#22417=CARTESIAN_POINT('Ctrl Pts',(1.02677414338759,-0.993235093958052,
1.41461332256796));
#22418=CARTESIAN_POINT('Ctrl Pts',(1.26586652272339,-0.985480669746802,
1.60644767971085));
#22419=CARTESIAN_POINT('Ctrl Pts',(1.5362079120753,-0.829355339157881,1.75614145458408));
#22420=CARTESIAN_POINT('Ctrl Pts',(0.830120749534202,-0.909788127533567,
1.13430117558029));
#22421=CARTESIAN_POINT('Ctrl Pts',(1.04293872696085,-1.0618660701672,1.35902160674438));
#22422=CARTESIAN_POINT('Ctrl Pts',(1.29215273573924,-1.06009969793961,1.54332567193682));
#22423=CARTESIAN_POINT('Ctrl Pts',(1.57786820262107,-0.904732449133388,
1.68715809360678));
#22424=CARTESIAN_POINT('Ctrl Pts',(0.834133632104406,-0.954061570898026,
1.10192284729582));
#22425=CARTESIAN_POINT('Ctrl Pts',(1.04975978886663,-1.115053684233,1.32027771712106));
#22426=CARTESIAN_POINT('Ctrl Pts',(1.30619109614144,-1.11871505289201,1.4993370241196));
#22427=CARTESIAN_POINT('Ctrl Pts',(1.60342755392884,-0.965045676875053,
1.63910076829144));
#22428=CARTESIAN_POINT('',(0.762735325532963,-0.766529441696069,1.28727233489076));
#22429=CARTESIAN_POINT('',(0.833432097145889,-0.946792943618195,1.10727038327973));
#22430=CARTESIAN_POINT('Ctrl Pts',(0.762735325532963,-0.766529441696069,
1.28727233489076));
#22431=CARTESIAN_POINT('Ctrl Pts',(0.788026430107248,-0.787197175676817,
1.25478273943462));
#22432=CARTESIAN_POINT('Ctrl Pts',(0.802282325162875,-0.810487357658538,
1.2282992378126));
#22433=CARTESIAN_POINT('Ctrl Pts',(0.822697729112149,-0.868959733809562,
1.17205963503304));
#22434=CARTESIAN_POINT('Ctrl Pts',(0.830470338502318,-0.904055468577785,
1.14130666672511));
#22435=CARTESIAN_POINT('Ctrl Pts',(0.833432097145889,-0.946792943618195,
1.10727038327973));
#22436=CARTESIAN_POINT('Ctrl Pts',(0.762735325532963,-0.766529441696069,
1.28727233489076));
#22437=CARTESIAN_POINT('Ctrl Pts',(0.847907059902912,-0.821288554787752,
1.39987124007464));
#22438=CARTESIAN_POINT('Ctrl Pts',(0.938212862837218,-0.849339599532016,
1.50346488650363));
#22439=CARTESIAN_POINT('Ctrl Pts',(1.15213731807335,-0.852349824604396,
1.715480776583));
#22440=CARTESIAN_POINT('Ctrl Pts',(1.27853461941729,-0.812854124246773,
1.81902921434248));
#22441=CARTESIAN_POINT('Ctrl Pts',(1.41284463836769,-0.732195474855993,
1.90869858745619));
#22442=CARTESIAN_POINT('Ctrl Pts',(0.833432097145889,-0.946792943618196,
1.10727038327973));
#22443=CARTESIAN_POINT('Ctrl Pts',(0.90381109288579,-0.996789604993471,
1.18103565901043));
#22444=CARTESIAN_POINT('Ctrl Pts',(0.983198189519679,-1.03588011685504,
1.25302429310888));
#22445=CARTESIAN_POINT('Ctrl Pts',(1.16484813617462,-1.07809517714267,1.39260788389877));
#22446=CARTESIAN_POINT('Ctrl Pts',(1.26249969691991,-1.07820617779495,1.4557470906386));
#22447=CARTESIAN_POINT('Ctrl Pts',(1.4421717994102,-1.03816533347022,1.55895701082589));
#22448=CARTESIAN_POINT('Ctrl Pts',(1.51906903401083,-1.00786966075201,1.5990490209941));
#22449=CARTESIAN_POINT('Ctrl Pts',(1.59279130921887,-0.967951970128402,
1.63615580822897));
#22450=CARTESIAN_POINT('Ctrl Pts',(1.04334803864883,-0.720016914634041,
1.10157231096021));
#22451=CARTESIAN_POINT('Ctrl Pts',(1.29208090893696,-0.823064346331372,
1.31988785480615));
#22452=CARTESIAN_POINT('Ctrl Pts',(1.54167481933163,-0.763481187915707,
1.49890963328679));
#22453=CARTESIAN_POINT('Ctrl Pts',(1.79212976983284,-0.541267439387045,
1.63863764640213));
#22454=CARTESIAN_POINT('Ctrl Pts',(0.99879485818792,-0.721111068024911,
1.13400885567558));
#22455=CARTESIAN_POINT('Ctrl Pts',(1.23841384267289,-0.826338820212016,
1.35870212368824));
#22456=CARTESIAN_POINT('Ctrl Pts',(1.48217213030307,-0.773689391859137,
1.54297833728479));
#22457=CARTESIAN_POINT('Ctrl Pts',(1.73011692219034,-0.56288064822183,1.68678245041579));
#22458=CARTESIAN_POINT('Ctrl Pts',(0.940500318558189,-0.71640818004708,
1.18052127745051));
#22459=CARTESIAN_POINT('Ctrl Pts',(1.16780827731181,-0.823317656434312,
1.4143978468945));
#22460=CARTESIAN_POINT('Ctrl Pts',(1.40296795752834,-0.778775904082548,
1.6062187263882));
#22461=CARTESIAN_POINT('Ctrl Pts',(1.64608829985706,-0.582659795462711,
1.75589536238257));
#22462=CARTESIAN_POINT('Ctrl Pts',(0.878650346215,-0.694504973991427,1.24109742378385));
#22463=CARTESIAN_POINT('Ctrl Pts',(1.09199968627953,-0.79959476424298,1.487102189602));
#22464=CARTESIAN_POINT('Ctrl Pts',(1.3154268563443,-0.76136977052119,1.6888313052158));
#22465=CARTESIAN_POINT('Ctrl Pts',(1.54892786092601,-0.579822225320567,
1.84628707150865));
#22466=CARTESIAN_POINT('Ctrl Pts',(0.856697251076076,-0.677918579829935,
1.26844862066248));
#22467=CARTESIAN_POINT('Ctrl Pts',(1.06477366572489,-0.780508474608168,
1.51987386218775));
#22468=CARTESIAN_POINT('Ctrl Pts',(1.28264229878622,-0.743414485344372,
1.72613059618618));
#22469=CARTESIAN_POINT('Ctrl Pts',(1.51049094310987,-0.566387689879693,
1.88706341654736));
#22470=CARTESIAN_POINT('Ctrl Pts',(0.846087143187382,-0.667616851769879,
1.28318517919043));
#22471=CARTESIAN_POINT('Ctrl Pts',(1.05147036139455,-0.768564946360839,
1.53754499301447));
#22472=CARTESIAN_POINT('Ctrl Pts',(1.26643337142018,-0.731592934569706,
1.7461278323729));
#22473=CARTESIAN_POINT('Ctrl Pts',(1.49097617326428,-0.556700816396479,
1.90893369726572));
#22474=CARTESIAN_POINT('',(0.849391336665505,-0.669228599956957,1.28727233489076));
#22475=CARTESIAN_POINT('Ctrl Pts',(1.03556549162895,-0.720159740047643,
1.10727038327973));
#22476=CARTESIAN_POINT('Ctrl Pts',(1.00975899746849,-0.720933639361777,
1.12801545944037));
#22477=CARTESIAN_POINT('Ctrl Pts',(0.981660765603823,-0.71995266969545,
1.15133239961421));
#22478=CARTESIAN_POINT('Ctrl Pts',(0.932697144981226,-0.712287980257606,
1.19509600545636));
#22479=CARTESIAN_POINT('Ctrl Pts',(0.913389476194193,-0.707566124812362,
1.21324740617548));
#22480=CARTESIAN_POINT('Ctrl Pts',(0.882563548282486,-0.694825406569064,
1.24538218411054));
#22481=CARTESIAN_POINT('Ctrl Pts',(0.866448281269861,-0.685758102882515,
1.26364457694964));
#22482=CARTESIAN_POINT('Ctrl Pts',(0.849391336665505,-0.669228599956958,
1.28727233489076));
#22483=CARTESIAN_POINT('Ctrl Pts',(0.849391336665505,-0.669228599956957,
1.28727233489076));
#22484=CARTESIAN_POINT('Ctrl Pts',(0.940530841324424,-0.713346345736857,
1.39987124007464));
#22485=CARTESIAN_POINT('Ctrl Pts',(1.03355488521186,-0.73033241101646,1.50346488650363));
#22486=CARTESIAN_POINT('Ctrl Pts',(1.2462884798982,-0.707591441492497,1.715480776583));
#22487=CARTESIAN_POINT('Ctrl Pts',(1.36701797678012,-0.653180259586498,
1.81902921434248));
#22488=CARTESIAN_POINT('Ctrl Pts',(1.49065195897357,-0.556953250077771,
1.90869858745619));
#22489=CARTESIAN_POINT('Ctrl Pts',(0.849391336665504,-0.669228599956957,
1.28727233489076));
#22490=CARTESIAN_POINT('Ctrl Pts',(1.05431200258793,-0.768424199911631,
1.54044292999952));
#22491=CARTESIAN_POINT('Ctrl Pts',(1.26875982659235,-0.730457460528791,
1.74808806061869));
#22492=CARTESIAN_POINT('Ctrl Pts',(1.49273480867877,-0.555328381808438,
1.91020772674828));
#22493=CARTESIAN_POINT('Ctrl Pts',(0.820505999621324,-0.701662213869995,
1.28727233489076));
#22494=CARTESIAN_POINT('Ctrl Pts',(1.02095396380933,-0.808833265245786,
1.54044292999951));
#22495=CARTESIAN_POINT('Ctrl Pts',(1.23640500988538,-0.779555824624012,
1.74808806061869));
#22496=CARTESIAN_POINT('Ctrl Pts',(1.46685913784949,-0.613829892004672,
1.91020772674828));
#22497=CARTESIAN_POINT('Ctrl Pts',(0.791620662577143,-0.734095827783032,
1.28727233489076));
#22498=CARTESIAN_POINT('Ctrl Pts',(0.98759592503072,-0.849242330579942,
1.54044292999952));
#22499=CARTESIAN_POINT('Ctrl Pts',(1.20405019317841,-0.828654188719233,
1.74808806061869));
#22500=CARTESIAN_POINT('Ctrl Pts',(1.4409834670202,-0.672331402200905,1.91020772674828));
#22501=CARTESIAN_POINT('Ctrl Pts',(0.762735325532963,-0.766529441696069,
1.28727233489076));
#22502=CARTESIAN_POINT('Ctrl Pts',(0.954237886252114,-0.889651395914097,
1.54044292999952));
#22503=CARTESIAN_POINT('Ctrl Pts',(1.17169537647143,-0.877752552814454,
1.74808806061869));
#22504=CARTESIAN_POINT('Ctrl Pts',(1.41510779619092,-0.730832912397139,
1.91020772674828));
#22505=CARTESIAN_POINT('Ctrl Pts',(0.849391336665504,-0.669228599956957,
1.28727233489076));
#22506=CARTESIAN_POINT('Ctrl Pts',(0.835451887202027,-0.68579028566881,
1.28797191329047));
#22507=CARTESIAN_POINT('Ctrl Pts',(0.821285101590925,-0.702160750604678,
1.28831907556383));
#22508=CARTESIAN_POINT('Ctrl Pts',(0.806883726521851,-0.718337308749603,
1.288319084765));
#22509=CARTESIAN_POINT('Ctrl Pts',(0.792392236721716,-0.734615089602759,
1.28831909402374));
#22510=CARTESIAN_POINT('Ctrl Pts',(0.777677820212489,-0.750680064449599,
1.28796761487395));
#22511=CARTESIAN_POINT('Ctrl Pts',(0.762735325532963,-0.766529441696069,
1.28727233489076));
#22512=CARTESIAN_POINT('Origin',(0.,0.,1.37171309575435));
#22513=CARTESIAN_POINT('',(0.762339710524744,-1.00491994924733,1.10727038327973));
#22514=CARTESIAN_POINT('Ctrl Pts',(1.52399042602929,-1.07301833748062,1.63615580822897));
#22515=CARTESIAN_POINT('Ctrl Pts',(1.42568690035943,-1.11607945894006,1.58735805514599));
#22516=CARTESIAN_POINT('Ctrl Pts',(1.33168344006445,-1.1415159485948,1.53858095020827));
#22517=CARTESIAN_POINT('Ctrl Pts',(1.14153741491427,-1.16157559133822,1.42806953503213));
#22518=CARTESIAN_POINT('Ctrl Pts',(1.04542790122454,-1.15142699410503,1.36461306044571));
#22519=CARTESIAN_POINT('Ctrl Pts',(0.882986840618225,-1.09387499947176,
1.23357020765531));
#22520=CARTESIAN_POINT('Ctrl Pts',(0.818276751491844,-1.05413090753297,
1.17136442658356));
#22521=CARTESIAN_POINT('Ctrl Pts',(0.762339710524743,-1.00491994924733,
1.10727038327973));
#22522=CARTESIAN_POINT('Origin',(0.,0.,1.10727038327973));
#22523=CARTESIAN_POINT('Ctrl Pts',(0.486216001172379,-0.96185791365589,
1.28318567027397));
#22524=CARTESIAN_POINT('Ctrl Pts',(0.629961036964703,-1.13989141130718,
1.53751096017972));
#22525=CARTESIAN_POINT('Ctrl Pts',(0.840463183520967,-1.19690070060403,
1.74607168007008));
#22526=CARTESIAN_POINT('Ctrl Pts',(1.11772244084117,-1.13288578154644,1.90886782994505));
#22527=CARTESIAN_POINT('Ctrl Pts',(0.494188516412735,-0.974277469399886,
1.26847940010162));
#22528=CARTESIAN_POINT('Ctrl Pts',(0.640136900598344,-1.15456280023806,
1.51987665322458));
#22529=CARTESIAN_POINT('Ctrl Pts',(0.853518266498016,-1.2119667709518,1.72611612827485));
#22530=CARTESIAN_POINT('Ctrl Pts',(1.13450705657511,-1.14670398409855,1.88704325648017));
#22531=CARTESIAN_POINT('Ctrl Pts',(0.506068912121111,-0.999036317271854,
1.24117979784214));
#22532=CARTESIAN_POINT('Ctrl Pts',(0.655595999565546,-1.18391556488183,
1.48716740433065));
#22533=CARTESIAN_POINT('Ctrl Pts',(0.87438875535233,-1.24297220725901,1.68888889262423));
#22534=CARTESIAN_POINT('Ctrl Pts',(1.16244328394297,-1.17621563803994,1.84634569530464));
#22535=CARTESIAN_POINT('Ctrl Pts',(0.515271549474752,-1.06384465023928,
1.18072830092662));
#22536=CARTESIAN_POINT('Ctrl Pts',(0.669593960494796,-1.26191264154004,
1.41461382576642));
#22537=CARTESIAN_POINT('Ctrl Pts',(0.899380393905811,-1.32842099300983,
1.60644836271615));
#22538=CARTESIAN_POINT('Ctrl Pts',(1.2047357142776,-1.26347706358718,1.75614213758938));
#22539=CARTESIAN_POINT('Ctrl Pts',(0.508351755467876,-1.12178134612809,
1.13430117558029));
#22540=CARTESIAN_POINT('Ctrl Pts',(0.66375901094087,-1.3321804361879,1.35902160674437));
#22541=CARTESIAN_POINT('Ctrl Pts',(0.901321456978324,-1.4075118803195,1.54332567193682));
#22542=CARTESIAN_POINT('Ctrl Pts',(1.22106413381299,-1.34803978074575,1.68715809360678));
#22543=CARTESIAN_POINT('Ctrl Pts',(0.498486987186291,-1.16512794184932,
1.10192284729582));
#22544=CARTESIAN_POINT('Ctrl Pts',(0.653810349677836,-1.38487268717996,
1.32027771712106));
#22545=CARTESIAN_POINT('Ctrl Pts',(0.896559590305321,-1.46759648753937,
1.4993370241196));
#22546=CARTESIAN_POINT('Ctrl Pts',(1.22673470906875,-1.41329934292755,1.63910076829144));
#22547=CARTESIAN_POINT('',(0.488533777383804,-0.964710998256926,1.28727233489076));
#22548=CARTESIAN_POINT('',(0.500065917147829,-1.15799828028599,1.10727038327973));
#22549=CARTESIAN_POINT('Ctrl Pts',(0.488533777383804,-0.964710998256926,
1.28727233489076));
#22550=CARTESIAN_POINT('Ctrl Pts',(0.506200366158218,-0.992182562456351,
1.2547827394346));
#22551=CARTESIAN_POINT('Ctrl Pts',(0.512561466011952,-1.01873815563797,
1.22829923781264));
#22552=CARTESIAN_POINT('Ctrl Pts',(0.513908711038643,-1.08065739676305,
1.17205963503661));
#22553=CARTESIAN_POINT('Ctrl Pts',(0.510455723375345,-1.11643729240063,
1.14130666672845));
#22554=CARTESIAN_POINT('Ctrl Pts',(0.500065917147829,-1.15799828028599,
1.10727038327973));
#22555=CARTESIAN_POINT('Ctrl Pts',(0.488533777383804,-0.964710998256926,
1.28727233489076));
#22556=CARTESIAN_POINT('Ctrl Pts',(0.552615413818274,-1.04310952295002,
1.39987124007464));
#22557=CARTESIAN_POINT('Ctrl Pts',(0.629833086622262,-1.09769367964031,
1.50346488650363));
#22558=CARTESIAN_POINT('Ctrl Pts',(0.832357123065218,-1.16666286599128,
1.715480776583));
#22559=CARTESIAN_POINT('Ctrl Pts',(0.964772942765736,-1.16815913695893,
1.81902921434248));
#22560=CARTESIAN_POINT('Ctrl Pts',(1.11743425489732,-1.13295228123076,1.90869858745619));
#22561=CARTESIAN_POINT('Ctrl Pts',(0.500065917147829,-1.15799828028599,
1.10727038327973));
#22562=CARTESIAN_POINT('Ctrl Pts',(0.551550501629604,-1.22729623661062,
1.18103565901044));
#22563=CARTESIAN_POINT('Ctrl Pts',(0.614972484708978,-1.28900548463583,
1.25302429310889));
#22564=CARTESIAN_POINT('Ctrl Pts',(0.774686679112385,-1.38528731335186,
1.39260788389878));
#22565=CARTESIAN_POINT('Ctrl Pts',(0.867524531197646,-1.41556887304305,
1.4557470906386));
#22566=CARTESIAN_POINT('Ctrl Pts',(1.05077615643295,-1.43300950021464,1.55895701082589));
#22567=CARTESIAN_POINT('Ctrl Pts',(1.13327165021091,-1.42795915557246,1.5990490209941));
#22568=CARTESIAN_POINT('Ctrl Pts',(1.21572094522251,-1.4127766116927,1.63615580822897));
#22569=CARTESIAN_POINT('Ctrl Pts',(0.769785488061416,-1.0071890534957,1.1015723109602));
#22570=CARTESIAN_POINT('Ctrl Pts',(0.974501097544584,-1.18205566887762,
1.31988785480615));
#22571=CARTESIAN_POINT('Ctrl Pts',(1.23029122098202,-1.2025174778094,1.4989096332868));
#22572=CARTESIAN_POINT('Ctrl Pts',(1.53715585837372,-1.06857448029103,1.63863764640215));
#22573=CARTESIAN_POINT('Ctrl Pts',(0.727074783470156,-0.994461965292039,
1.13400885567557));
#22574=CARTESIAN_POINT('Ctrl Pts',(0.922448816386937,-1.16858584308541,
1.35870212368824));
#22575=CARTESIAN_POINT('Ctrl Pts',(1.17054629234374,-1.19383871456864,1.5429783372848));
#22576=CARTESIAN_POINT('Ctrl Pts',(1.47149928669635,-1.06996683960028,1.6867824504158));
#22577=CARTESIAN_POINT('Ctrl Pts',(0.673083751047337,-0.971974682567371,
1.18052322600158));
#22578=CARTESIAN_POINT('Ctrl Pts',(0.856229621362344,-1.14389365895071,
1.41439979544558));
#22579=CARTESIAN_POINT('Ctrl Pts',(1.09364268483531,-1.17420151395341,1.60622137130567));
#22580=CARTESIAN_POINT('Ctrl Pts',(1.38546708108518,-1.06281232835787,1.75589800730004));
#22581=CARTESIAN_POINT('Ctrl Pts',(0.621030952892817,-0.932030917609336,
1.24109849008298));
#22582=CARTESIAN_POINT('Ctrl Pts',(0.791463701885441,-1.09790581924279,
1.48710325590114));
#22583=CARTESIAN_POINT('Ctrl Pts',(1.01576709402368,-1.13059499103696,1.68883275601271));
#22584=CARTESIAN_POINT('Ctrl Pts',(1.29394102274665,-1.03008879377587,1.84628852230557));
#22585=CARTESIAN_POINT('Ctrl Pts',(0.605279141158067,-0.909472892481624,
1.26844862066248));
#22586=CARTESIAN_POINT('Ctrl Pts',(0.771469550259553,-1.0713408286716,1.51987386218776));
#22587=CARTESIAN_POINT('Ctrl Pts',(0.990137606500536,-1.10338745862407,
1.7261305961862));
#22588=CARTESIAN_POINT('Ctrl Pts',(1.26153883267191,-1.00543407447982,1.88706341654738));
#22589=CARTESIAN_POINT('Ctrl Pts',(0.598371737953918,-0.89639666323125,
1.28318517919043));
#22590=CARTESIAN_POINT('Ctrl Pts',(0.762508109189142,-1.055870911185,1.53754499301449));
#22591=CARTESIAN_POINT('Ctrl Pts',(0.978375060596146,-1.08713566171041,
1.74612783237293));
#22592=CARTESIAN_POINT('Ctrl Pts',(1.24597259217493,-0.990190914807476,
1.90893369726575));
#22593=CARTESIAN_POINT('',(0.601016155111926,-0.89895057878464,1.28727233489076));
#22594=CARTESIAN_POINT('Ctrl Pts',(0.762339710524743,-1.00491994924733,
1.10727038327973));
#22595=CARTESIAN_POINT('Ctrl Pts',(0.737557128050331,-0.997681325972066,
1.12801545944067));
#22596=CARTESIAN_POINT('Ctrl Pts',(0.711137257837026,-0.98806553722051,
1.15133239961449));
#22597=CARTESIAN_POINT('Ctrl Pts',(0.666938606675585,-0.965645393506861,
1.19509600545645));
#22598=CARTESIAN_POINT('Ctrl Pts',(0.650035056038514,-0.955188244339448,
1.21324740617592));
#22599=CARTESIAN_POINT('Ctrl Pts',(0.624654954884888,-0.933545365639724,
1.24538218411107));
#22600=CARTESIAN_POINT('Ctrl Pts',(0.612130376113162,-0.919941956007489,
1.26364457695018));
#22601=CARTESIAN_POINT('Ctrl Pts',(0.601016155111926,-0.89895057878464,
1.28727233489076));
#22602=CARTESIAN_POINT('Ctrl Pts',(0.601016155111926,-0.89895057878464,
1.28727233489076));
#22603=CARTESIAN_POINT('Ctrl Pts',(0.674061841710201,-0.969072704191387,
1.39987124007464));
#22604=CARTESIAN_POINT('Ctrl Pts',(0.757283981982513,-1.01397342270847,
1.50346488650363));
#22605=CARTESIAN_POINT('Ctrl Pts',(0.966632999495317,-1.05808377148838,
1.715480776583));
#22606=CARTESIAN_POINT('Ctrl Pts',(1.09826755410688,-1.04364312863621,1.81902921434248));
#22607=CARTESIAN_POINT('Ctrl Pts',(1.24558623976355,-0.990330805779366,
1.90869858745619));
#22608=CARTESIAN_POINT('Ctrl Pts',(0.601016155111926,-0.89895057878464,
1.28727233489076));
#22609=CARTESIAN_POINT('Ctrl Pts',(0.765254163607779,-1.056615168778,1.54044292999952));
#22610=CARTESIAN_POINT('Ctrl Pts',(0.980938531722803,-1.08677467590956,
1.74808806061869));
#22611=CARTESIAN_POINT('Ctrl Pts',(1.248069259457,-0.989429100179332,1.91020772674828));
#22612=CARTESIAN_POINT('Ctrl Pts',(0.563522029202552,-0.920870718608735,
1.28727233489076));
#22613=CARTESIAN_POINT('Ctrl Pts',(0.721041695541498,-1.08473827279984,
1.54044292999952));
#22614=CARTESIAN_POINT('Ctrl Pts',(0.934995043558668,-1.12347180680942,
1.74808806061869));
#22615=CARTESIAN_POINT('Ctrl Pts',(1.20538207325406,-1.03707132063747,1.91020772674828));
#22616=CARTESIAN_POINT('Ctrl Pts',(0.526027903293178,-0.942790858432831,
1.28727233489076));
#22617=CARTESIAN_POINT('Ctrl Pts',(0.676829227475217,-1.11286137682168,
1.54044292999952));
#22618=CARTESIAN_POINT('Ctrl Pts',(0.889051555394535,-1.16016893770927,
1.74808806061869));
#22619=CARTESIAN_POINT('Ctrl Pts',(1.16269488705113,-1.0847135410956,1.91020772674828));
#22620=CARTESIAN_POINT('Ctrl Pts',(0.488533777383804,-0.964710998256926,
1.28727233489076));
#22621=CARTESIAN_POINT('Ctrl Pts',(0.632616759408936,-1.14098448084351,
1.54044292999952));
#22622=CARTESIAN_POINT('Ctrl Pts',(0.843108067230401,-1.19686606860912,
1.74808806061869));
#22623=CARTESIAN_POINT('Ctrl Pts',(1.1200077008482,-1.13235576155374,1.91020772674828));
#22624=CARTESIAN_POINT('Ctrl Pts',(0.601016155111926,-0.89895057878464,
1.28727233489076));
#22625=CARTESIAN_POINT('Ctrl Pts',(0.582641108525679,-0.910394151125273,
1.28797191329046));
#22626=CARTESIAN_POINT('Ctrl Pts',(0.564108942884271,-0.92158561096782,
1.28831907556383));
#22627=CARTESIAN_POINT('Ctrl Pts',(0.545413589903933,-0.932520162364074,
1.288319084765));
#22628=CARTESIAN_POINT('Ctrl Pts',(0.526601253184352,-0.94352313529324,
1.28831909402374));
#22629=CARTESIAN_POINT('Ctrl Pts',(0.50764266123789,-0.954254829541782,
1.28796761487395));
#22630=CARTESIAN_POINT('Ctrl Pts',(0.488533777383804,-0.964710998256926,
1.28727233489076));
#22631=CARTESIAN_POINT('Origin',(0.,0.,1.37171309575435));
#22632=CARTESIAN_POINT('',(0.414490807021285,-1.19131159212569,1.10727038327973));
#22633=CARTESIAN_POINT('Ctrl Pts',(1.11782012388912,-1.4914400228729,1.63615580822897));
#22634=CARTESIAN_POINT('Ctrl Pts',(1.01102129689823,-1.50201612299692,1.587358055146));
#22635=CARTESIAN_POINT('Ctrl Pts',(0.913758385849818,-1.49715899547354,
1.53858095020828));
#22636=CARTESIAN_POINT('Ctrl Pts',(0.72671999907427,-1.45747849623495,1.42806953503211));
#22637=CARTESIAN_POINT('Ctrl Pts',(0.638450508815826,-1.41812713365383,
1.36461306044569));
#22638=CARTESIAN_POINT('Ctrl Pts',(0.501744424014166,-1.31319488582044,
1.2335702076553));
#22639=CARTESIAN_POINT('Ctrl Pts',(0.452483071915568,-1.25539949095026,
1.17136442658355));
#22640=CARTESIAN_POINT('Ctrl Pts',(0.414490807021284,-1.19131159212569,
1.10727038327973));
#22641=CARTESIAN_POINT('Origin',(0.,0.,1.10727038327973));
#22642=CARTESIAN_POINT('Ctrl Pts',(0.165188454748262,-1.06503024383179,
1.28318567027397));
#22643=CARTESIAN_POINT('Ctrl Pts',(0.246882731381369,-1.27876982080873,
1.53751096017971));
#22644=CARTESIAN_POINT('Ctrl Pts',(0.429465330327856,-1.39803761752215,
1.74607168007008));
#22645=CARTESIAN_POINT('Ctrl Pts',(0.712936251587724,-1.42283363397204,
1.90886782994505));
#22646=CARTESIAN_POINT('Ctrl Pts',(0.168932913531383,-1.07930558594879,
1.26847940010162));
#22647=CARTESIAN_POINT('Ctrl Pts',(0.252026844288349,-1.29586765564978,
1.51987665322458));
#22648=CARTESIAN_POINT('Ctrl Pts',(0.437225780288044,-1.41640054440424,
1.72611612827484));
#22649=CARTESIAN_POINT('Ctrl Pts',(0.724629310334678,-1.44116225705855,
1.88704325648017));
#22650=CARTESIAN_POINT('Ctrl Pts',(0.172580460092752,-1.10652474870095,
1.24117906537517));
#22651=CARTESIAN_POINT('Ctrl Pts',(0.257658341550682,-1.32856177300787,
1.48716667186368));
#22652=CARTESIAN_POINT('Ctrl Pts',(0.447493258920482,-1.45233913898616,
1.68888789608759));
#22653=CARTESIAN_POINT('Ctrl Pts',(0.742078309759795,-1.47786361346603,
1.846344698768));
#22654=CARTESIAN_POINT('Ctrl Pts',(0.161305070542798,-1.171005693206,1.18072695962337));
#22655=CARTESIAN_POINT('Ctrl Pts',(0.246868029800146,-1.40706779462018,
1.41461248446318));
#22656=CARTESIAN_POINT('Ctrl Pts',(0.444855864337698,-1.54132997390971,
1.60644654213682));
#22657=CARTESIAN_POINT('Ctrl Pts',(0.755334809435768,-1.57392460995617,
1.75614031701005));
#22658=CARTESIAN_POINT('Ctrl Pts',(0.136821749681419,-1.22396679065339,
1.13430117558029));
#22659=CARTESIAN_POINT('Ctrl Pts',(0.219605938249048,-1.47209169926767,
1.35902160674437));
#22660=CARTESIAN_POINT('Ctrl Pts',(0.422262554132511,-1.61714699314179,
1.54332567193682));
#22661=CARTESIAN_POINT('Ctrl Pts',(0.744733799933223,-1.65939158627327,
1.68715809360678));
#22662=CARTESIAN_POINT('Ctrl Pts',(0.114044962799315,-1.26214347192869,
1.10192284729582));
#22663=CARTESIAN_POINT('Ctrl Pts',(0.193861398098011,-1.51913070253035,
1.32027771712106));
#22664=CARTESIAN_POINT('Ctrl Pts',(0.399166585072141,-1.67281935264038,
1.4993370241196));
#22665=CARTESIAN_POINT('Ctrl Pts',(0.729960523721706,-1.72320942225876,
1.63910076829143));
#22666=CARTESIAN_POINT('',(0.166511139289342,-1.06845992077163,1.28727233489076));
#22667=CARTESIAN_POINT('',(0.117749801015222,-1.25585067703094,1.10727038327973));
#22668=CARTESIAN_POINT('Ctrl Pts',(0.166511139289342,-1.06845992077163,
1.28727233489076));
#22669=CARTESIAN_POINT('Ctrl Pts',(0.174823883464339,-1.10004620708051,
1.25478273943433));
#22670=CARTESIAN_POINT('Ctrl Pts',(0.17266751934213,-1.12726776497774,1.22829923781233));
#22671=CARTESIAN_POINT('Ctrl Pts',(0.154814727716273,-1.18657278434574,
1.17205963503338));
#22672=CARTESIAN_POINT('Ctrl Pts',(0.140474145488556,-1.21953445537463,
1.14130666672549));
#22673=CARTESIAN_POINT('Ctrl Pts',(0.117749801015222,-1.25585067703094,
1.10727038327973));
#22674=CARTESIAN_POINT('Ctrl Pts',(0.166511139289342,-1.06845992077163,
1.28727233489076));
#22675=CARTESIAN_POINT('Ctrl Pts',(0.203229920731113,-1.16282366323453,
1.39987124007464));
#22676=CARTESIAN_POINT('Ctrl Pts',(0.259800859583567,-1.23859785430383,
1.50346488650363));
#22677=CARTESIAN_POINT('Ctrl Pts',(0.431100013478375,-1.36677481743678,
1.715480776583));
#22678=CARTESIAN_POINT('Ctrl Pts',(0.556572568507924,-1.40911659430226,
1.81902921434248));
#22679=CARTESIAN_POINT('Ctrl Pts',(0.712641620935351,-1.42280782457595,
1.90869858745619));
#22680=CARTESIAN_POINT('Ctrl Pts',(0.117749801015222,-1.25585067703094,
1.10727038327973));
#22681=CARTESIAN_POINT('Ctrl Pts',(0.145300304395592,-1.33766656151261,
1.18103565901042));
#22682=CARTESIAN_POINT('Ctrl Pts',(0.18654898832969,-1.41595401455113,1.25302429310886));
#22683=CARTESIAN_POINT('Ctrl Pts',(0.308693492339104,-1.55687787546587,
1.39260788389873));
#22684=CARTESIAN_POINT('Ctrl Pts',(0.387630019962874,-1.61436582414938,
1.45574709063857));
#22685=CARTESIAN_POINT('Ctrl Pts',(0.556523222076021,-1.68758071271375,
1.55895701082587));
#22686=CARTESIAN_POINT('Ctrl Pts',(0.636541741320434,-1.70827005906903,
1.59904902099409));
#22687=CARTESIAN_POINT('Ctrl Pts',(0.71964734468187,-1.71930883511106,1.63615580822897));
#22688=CARTESIAN_POINT('Ctrl Pts',(0.420870970491666,-1.19577051030242,
1.1015723109602));
#22689=CARTESIAN_POINT('Ctrl Pts',(0.561530328976117,-1.425339146688,1.31988785480614));
#22690=CARTESIAN_POINT('Ctrl Pts',(0.798478145979644,-1.52384297854318,
1.49890963328679));
#22691=CARTESIAN_POINT('Ctrl Pts',(1.13171442150225,-1.49128200586798,1.63863764640213));
#22692=CARTESIAN_POINT('Ctrl Pts',(0.384183563118433,-1.17046799657245,
1.13400885567557));
#22693=CARTESIAN_POINT('Ctrl Pts',(0.516188072874178,-1.39644354162126,
1.35870212368824));
#22694=CARTESIAN_POINT('Ctrl Pts',(0.744339227614173,-1.49712678593272,
1.54297833728479));
#22695=CARTESIAN_POINT('Ctrl Pts',(1.06884104848206,-1.47231722182136,1.68678245041579));
#22696=CARTESIAN_POINT('Ctrl Pts',(0.339783831202729,-1.13239708355232,
1.18052334762519));
#22697=CARTESIAN_POINT('Ctrl Pts',(0.460840019240362,-1.3524969326934,1.41439991706918));
#22698=CARTESIAN_POINT('Ctrl Pts',(0.677267520477999,-1.45468613664231,
1.60622153639668));
#22699=CARTESIAN_POINT('Ctrl Pts',(0.989230165483925,-1.43892742365129,
1.75589817239104));
#22700=CARTESIAN_POINT('Ctrl Pts',(0.302622070510769,-1.07832314329337,
1.24109855662706));
#22701=CARTESIAN_POINT('Ctrl Pts',(0.413455083485284,-1.28874616521844,
1.48710332244522));
#22702=CARTESIAN_POINT('Ctrl Pts',(0.61667872836244,-1.38914899293201,1.68883284655014));
#22703=CARTESIAN_POINT('Ctrl Pts',(0.912295978931507,-1.37952239046626,
1.846288612843));
#22704=CARTESIAN_POINT('Ctrl Pts',(0.294612091675752,-1.05200166174697,
1.26844862066248));
#22705=CARTESIAN_POINT('Ctrl Pts',(0.402648620070371,-1.25730287795417,
1.51987386218775));
#22706=CARTESIAN_POINT('Ctrl Pts',(0.600711346596184,-1.35535317970116,
1.72613059618619));
#22707=CARTESIAN_POINT('Ctrl Pts',(0.889098511634057,-1.34606156659877,
1.88706341654736));
#22708=CARTESIAN_POINT('Ctrl Pts',(0.292083537908477,-1.03743092373275,
1.28318517919043));
#22709=CARTESIAN_POINT('Ctrl Pts',(0.3989062505499,-1.23982087453714,1.53754499301448));
#22710=CARTESIAN_POINT('Ctrl Pts',(0.594546582101045,-1.33626197576335,
1.74612783237291));
#22711=CARTESIAN_POINT('Ctrl Pts',(0.879004532561912,-1.32675422741137,
1.90893369726573));
#22712=CARTESIAN_POINT('',(0.293809324770207,-1.04067701160391,1.28727233489076));
#22713=CARTESIAN_POINT('Ctrl Pts',(0.414490807021284,-1.19131159212569,
1.10727038327973));
#22714=CARTESIAN_POINT('Ctrl Pts',(0.393158028076601,-1.17676901314185,
1.12801545944039));
#22715=CARTESIAN_POINT('Ctrl Pts',(0.371002680489087,-1.15945966570535,
1.15133239961415));
#22716=CARTESIAN_POINT('Ctrl Pts',(0.335895470715215,-1.12447870759369,
1.19509600545509));
#22717=CARTESIAN_POINT('Ctrl Pts',(0.323050675538403,-1.10930988332415,
1.21324740617454));
#22718=CARTESIAN_POINT('Ctrl Pts',(0.30560078227685,-1.08088339992903,1.24538218411075));
#22719=CARTESIAN_POINT('Ctrl Pts',(0.297892884779821,-1.06407548086656,
1.26364457694995));
#22720=CARTESIAN_POINT('Ctrl Pts',(0.293809324770207,-1.04067701160391,
1.28727233489076));
#22721=CARTESIAN_POINT('Ctrl Pts',(0.293809324770207,-1.04067701160391,
1.28727233489076));
#22722=CARTESIAN_POINT('Ctrl Pts',(0.341610972564374,-1.12993947443311,
1.39987124007464));
#22723=CARTESIAN_POINT('Ctrl Pts',(0.406884846288962,-1.19835965101752,
1.50346488650363));
#22724=CARTESIAN_POINT('Ctrl Pts',(0.592356746173702,-1.30500348982786,
1.715480776583));
#22725=CARTESIAN_POINT('Ctrl Pts',(0.722011051157661,-1.33194693676576,
1.81902921434248));
#22726=CARTESIAN_POINT('Ctrl Pts',(0.878593860895847,-1.32676788217082,
1.90869858745619));
#22727=CARTESIAN_POINT('Ctrl Pts',(0.293809324770207,-1.04067701160391,
1.28727233489076));
#22728=CARTESIAN_POINT('Ctrl Pts',(0.401287915254421,-1.24137728305361,
1.54044292999952));
#22729=CARTESIAN_POINT('Ctrl Pts',(0.59709613876759,-1.3367108140079,1.74808806061869));
#22730=CARTESIAN_POINT('Ctrl Pts',(0.881233995309716,-1.32667760446677,
1.91020772674828));
#22731=CARTESIAN_POINT('Ctrl Pts',(0.251376596276585,-1.04993798132648,
1.28727233489076));
#22732=CARTESIAN_POINT('Ctrl Pts',(0.350548842321171,-1.25446154039629,
1.54044292999952));
#22733=CARTESIAN_POINT('Ctrl Pts',(0.542061247874906,-1.35741454085596,
1.74808806061869));
#22734=CARTESIAN_POINT('Ctrl Pts',(0.825913812937791,-1.3587969827055,1.91020772674828));
#22735=CARTESIAN_POINT('Ctrl Pts',(0.208943867782964,-1.05919895104906,
1.28727233489076));
#22736=CARTESIAN_POINT('Ctrl Pts',(0.29980976938792,-1.26754579773896,1.54044292999952));
#22737=CARTESIAN_POINT('Ctrl Pts',(0.487026356982221,-1.37811826770402,
1.74808806061869));
#22738=CARTESIAN_POINT('Ctrl Pts',(0.770593630565866,-1.39091636094422,
1.91020772674828));
#22739=CARTESIAN_POINT('Ctrl Pts',(0.166511139289342,-1.06845992077163,
1.28727233489076));
#22740=CARTESIAN_POINT('Ctrl Pts',(0.24907069645467,-1.28063005508163,1.54044292999952));
#22741=CARTESIAN_POINT('Ctrl Pts',(0.431991466089537,-1.39882199455207,
1.74808806061869));
#22742=CARTESIAN_POINT('Ctrl Pts',(0.715273448193942,-1.42303573918295,
1.91020772674828));
#22743=CARTESIAN_POINT('Ctrl Pts',(0.293809324770207,-1.04067701160391,
1.28727233489076));
#22744=CARTESIAN_POINT('Ctrl Pts',(0.272797358647511,-1.04588229398058,
1.28797191329046));
#22745=CARTESIAN_POINT('Ctrl Pts',(0.25171387046998,-1.05079925066492,1.28831907556383));
#22746=CARTESIAN_POINT('Ctrl Pts',(0.230554570986284,-1.05542144523633,
1.288319084765));
#22747=CARTESIAN_POINT('Ctrl Pts',(0.209262869938635,-1.06007256258898,
1.28831909402374));
#22748=CARTESIAN_POINT('Ctrl Pts',(0.187915901626942,-1.06442048323406,
1.28796761487395));
#22749=CARTESIAN_POINT('Ctrl Pts',(0.166511139289342,-1.06845992077163,
1.28727233489076));
#22750=CARTESIAN_POINT('Origin',(0.,0.,1.37171309575435));
#22751=CARTESIAN_POINT('',(0.0260686553993157,-1.26108935601086,1.10727038327973));
#22752=CARTESIAN_POINT('Ctrl Pts',(0.602229799711917,-1.76386916735272,
1.63615580822897));
#22753=CARTESIAN_POINT('Ctrl Pts',(0.497389884697426,-1.74092498377324,
1.58735805514619));
#22754=CARTESIAN_POINT('Ctrl Pts',(0.406388294299505,-1.70624968855542,
1.53858095020849));
#22755=CARTESIAN_POINT('Ctrl Pts',(0.240766166369039,-1.61071325107048,
1.42806953503218));
#22756=CARTESIAN_POINT('Ctrl Pts',(0.168977132258039,-1.54601110868793,
1.36461306044575));
#22757=CARTESIAN_POINT('Ctrl Pts',(0.071387767328661,-1.40397010717828,
1.23357020765533));
#22758=CARTESIAN_POINT('Ctrl Pts',(0.0423971966252674,-1.33378082531077,
1.17136442658357));
#22759=CARTESIAN_POINT('Ctrl Pts',(0.0260686553993153,-1.26108935601086,
1.10727038327973));
#22760=CARTESIAN_POINT('Origin',(0.,0.,1.10727038327973));
#22761=CARTESIAN_POINT('Ctrl Pts',(-0.172008888562255,-1.06394999323939,
1.28318567027397));
#22762=CARTESIAN_POINT('Ctrl Pts',(-0.160362439116273,-1.2924681694826,
1.5375052164054));
#22763=CARTESIAN_POINT('Ctrl Pts',(-0.023577760251312,-1.46231719972917,
1.74606225962531));
#22764=CARTESIAN_POINT('Ctrl Pts',(0.238345148032627,-1.57349708397912,
1.90885679993368));
#22765=CARTESIAN_POINT('Ctrl Pts',(-0.173142620221682,-1.08359887191535,
1.26357344997188));
#22766=CARTESIAN_POINT('Ctrl Pts',(-0.160807978363557,-1.31626526877614,
1.51398865241804));
#22767=CARTESIAN_POINT('Ctrl Pts',(-0.0213345743744544,-1.48889372807638,
1.71944966391904));
#22768=CARTESIAN_POINT('Ctrl Pts',(0.245622116073242,-1.601562386112,1.87975180733571));
#22769=CARTESIAN_POINT('Ctrl Pts',(-0.181917271417173,-1.11842748291058,
1.2281366482377));
#22770=CARTESIAN_POINT('Ctrl Pts',(-0.169920645136297,-1.35874448434795,
1.47149643610478));
#22771=CARTESIAN_POINT('Ctrl Pts',(-0.0262779583676895,-1.53749711063698,
1.6710635087107));
#22772=CARTESIAN_POINT('Ctrl Pts',(0.249006836337355,-1.6546951488403,1.82683387344445));
#22773=CARTESIAN_POINT('Ctrl Pts',(-0.219636735943001,-1.1753425954218,
1.16789882161102));
#22774=CARTESIAN_POINT('Ctrl Pts',(-0.21298531416801,-1.42921995625554,
1.39924604542984));
#22775=CARTESIAN_POINT('Ctrl Pts',(-0.0659764462771748,-1.62139761687088,
1.58900346231478));
#22776=CARTESIAN_POINT('Ctrl Pts',(0.221543302854981,-1.75191643683035,
1.73707641259309));
#22777=CARTESIAN_POINT('Ctrl Pts',(-0.256493105922012,-1.21368608666858,
1.126177305135));
#22778=CARTESIAN_POINT('Ctrl Pts',(-0.255772600666387,-1.47711033277873,
1.34930521631815));
#22779=CARTESIAN_POINT('Ctrl Pts',(-0.107970878520535,-1.6800421801244,
1.53227487652584));
#22780=CARTESIAN_POINT('Ctrl Pts',(0.187015176303949,-1.82238303426191,
1.67509057207931));
#22781=CARTESIAN_POINT('Ctrl Pts',(-0.281595159362693,-1.235641855012,1.10188938448118));
#22782=CARTESIAN_POINT('Ctrl Pts',(-0.285104353628414,-1.50471757474417,
1.32023273220193));
#22783=CARTESIAN_POINT('Ctrl Pts',(-0.137346783688564,-1.71433282083683,
1.49928348142626));
#22784=CARTESIAN_POINT('Ctrl Pts',(0.161677550456857,-1.86448759328998,
1.63904163215416));
#22785=CARTESIAN_POINT('',(-0.171810769270086,-1.06762054184321,1.28727233489076));
#22786=CARTESIAN_POINT('',(-0.27609248605186,-1.23077165948193,1.10727038327973));
#22787=CARTESIAN_POINT('Ctrl Pts',(-0.171810769270086,-1.06762054184321,
1.28727233489076));
#22788=CARTESIAN_POINT('Ctrl Pts',(-0.173665579012837,-1.10022966448349,
1.25478273943364));
#22789=CARTESIAN_POINT('Ctrl Pts',(-0.184128327166747,-1.12545255134542,
1.22829923781169));
#22790=CARTESIAN_POINT('Ctrl Pts',(-0.219433599813331,-1.1763381604554,
1.17205963503223));
#22791=CARTESIAN_POINT('Ctrl Pts',(-0.24325802049969,-1.20325508885762,
1.14130666672443));
#22792=CARTESIAN_POINT('Ctrl Pts',(-0.27609248605186,-1.23077165948193,
1.10727038327973));
#22793=CARTESIAN_POINT('Ctrl Pts',(-0.171810769270086,-1.06762054184321,
1.28727233489076));
#22794=CARTESIAN_POINT('Ctrl Pts',(-0.166049132983329,-1.16871252149279,
1.39987124007464));
#22795=CARTESIAN_POINT('Ctrl Pts',(-0.135662485730196,-1.2582594411694,
1.50346488650363));
#22796=CARTESIAN_POINT('Ctrl Pts',(-0.0123561690781442,-1.43309732687145,
1.715480776583));
#22797=CARTESIAN_POINT('Ctrl Pts',(0.0938909933754464,-1.51213990150266,
1.81902921434248));
#22798=CARTESIAN_POINT('Ctrl Pts',(0.238090659850087,-1.57338902476662,
1.90869858745619));
#22799=CARTESIAN_POINT('Ctrl Pts',(-0.27609248605186,-1.23077165948193,
1.10727038327973));
#22800=CARTESIAN_POINT('Ctrl Pts',(-0.275172898999399,-1.31709676330278,
1.18103565901041));
#22801=CARTESIAN_POINT('Ctrl Pts',(-0.260135222790515,-1.40429909999044,
1.25302429310884));
#22802=CARTESIAN_POINT('Ctrl Pts',(-0.189563202796486,-1.57122974978687,
1.38867432147861));
#22803=CARTESIAN_POINT('Ctrl Pts',(-0.136388204217752,-1.64657149028472,
1.44891114041811));
#22804=CARTESIAN_POINT('Ctrl Pts',(-0.00179051121356718,-1.77077010917836,
1.55340617058598));
#22805=CARTESIAN_POINT('Ctrl Pts',(0.0722162251277554,-1.81883456875388,
1.59645518670945));
#22806=CARTESIAN_POINT('Ctrl Pts',(0.153129647965885,-1.85754313061971,
1.63615580822897));
#22807=CARTESIAN_POINT('Ctrl Pts',(0.0307586699497045,-1.26730161813769,
1.10157231096021));
#22808=CARTESIAN_POINT('Ctrl Pts',(0.0935930593956122,-1.52910049789876,
1.31988785480616));
#22809=CARTESIAN_POINT('Ctrl Pts',(0.288504466724427,-1.69600411129882,
1.49890963328681));
#22810=CARTESIAN_POINT('Ctrl Pts',(0.615492891936149,-1.76801245833785,
1.63863764640215));
#22811=CARTESIAN_POINT('Ctrl Pts',(0.0104540016207175,-1.24075075344812,
1.12589971949673));
#22812=CARTESIAN_POINT('Ctrl Pts',(0.0678859432465663,-1.4979766733267,
1.34900830339198));
#22813=CARTESIAN_POINT('Ctrl Pts',(0.256119480862723,-1.66433379116766,
1.53195557707746));
#22814=CARTESIAN_POINT('Ctrl Pts',(0.575041124025717,-1.73991331668443,
1.6747462494124));
#22815=CARTESIAN_POINT('Ctrl Pts',(-0.0181391694102216,-1.19576910668283,
1.16769197379075));
#22816=CARTESIAN_POINT('Ctrl Pts',(0.031367240156502,-1.44497975845611,
1.39903467275813));
#22817=CARTESIAN_POINT('Ctrl Pts',(0.208916886053918,-1.60956344041242,
1.58878224232002));
#22818=CARTESIAN_POINT('Ctrl Pts',(0.514553591586042,-1.68965392328532,
1.73683914729674));
#22819=CARTESIAN_POINT('Ctrl Pts',(-0.0438923944102224,-1.13237144427268,
1.22804151155252));
#22820=CARTESIAN_POINT('Ctrl Pts',(-0.00259486397362604,-1.36948062872853,
1.47142038155714));
#22821=CARTESIAN_POINT('Ctrl Pts',(0.161878639424902,-1.52936917527703,
1.67099694623233));
#22822=CARTESIAN_POINT('Ctrl Pts',(0.449540694258314,-1.61203607707659,
1.82676565001254));
#22823=CARTESIAN_POINT('Ctrl Pts',(-0.0455929113995308,-1.09643283244092,
1.2635364344865));
#22824=CARTESIAN_POINT('Ctrl Pts',(-0.00627769421187312,-1.32612616419273,
1.51398418220584));
#22825=CARTESIAN_POINT('Ctrl Pts',(0.152505158025993,-1.48124586260132,
1.71946457116169));
#22826=CARTESIAN_POINT('Ctrl Pts',(0.430838249779537,-1.56208770129018,
1.87977332297458));
#22827=CARTESIAN_POINT('Ctrl Pts',(-0.042795833893119,-1.07691421721301,
1.28318517919043));
#22828=CARTESIAN_POINT('Ctrl Pts',(-0.00374333123643638,-1.30240853234962,
1.53754499301448));
#22829=CARTESIAN_POINT('Ctrl Pts',(0.152519741700297,-1.45458565734394,
1.74612783237292));
#22830=CARTESIAN_POINT('Ctrl Pts',(0.425993384917082,-1.53344559219597,
1.90893369726574));
#22831=CARTESIAN_POINT('',(-0.0421576093699572,-1.08053472770428,1.28727233489076));
#22832=CARTESIAN_POINT('Ctrl Pts',(0.0260686553993155,-1.26108935601086,
1.10727038327973));
#22833=CARTESIAN_POINT('Ctrl Pts',(0.0102738810212638,-1.2406663502733,
1.12801545944049));
#22834=CARTESIAN_POINT('Ctrl Pts',(-0.00544822415320455,-1.21735780368012,
1.15133239961429));
#22835=CARTESIAN_POINT('Ctrl Pts',(-0.0280274542414684,-1.17324021107675,
1.19509600545504));
#22836=CARTESIAN_POINT('Ctrl Pts',(-0.0355561559109315,-1.15484454191159,
1.21324740617467));
#22837=CARTESIAN_POINT('Ctrl Pts',(-0.0433677241466708,-1.12241703607508,
1.24538218411125));
#22838=CARTESIAN_POINT('Ctrl Pts',(-0.0455044376575851,-1.10404988380792,
1.26364457695041));
#22839=CARTESIAN_POINT('Ctrl Pts',(-0.0421576093699572,-1.08053472770428,
1.28727233489076));
#22840=CARTESIAN_POINT('Ctrl Pts',(-0.0421576093699572,-1.08053472770428,
1.28727233489076));
#22841=CARTESIAN_POINT('Ctrl Pts',(-0.024279158719655,-1.18019989616608,
1.39987124007464));
#22842=CARTESIAN_POINT('Ctrl Pts',(0.0166569869072255,-1.26544208722232,
1.50346488650363));
#22843=CARTESIAN_POINT('Ctrl Pts',(0.16009648734447,-1.42418037408903,1.715480776583));
#22844=CARTESIAN_POINT('Ctrl Pts',(0.275079075974332,-1.48987049850469,
1.81902921434248));
#22845=CARTESIAN_POINT('Ctrl Pts',(0.425598593400271,-1.53333167412,1.90869858745619));
#22846=CARTESIAN_POINT('Ctrl Pts',(-0.0421576093699572,-1.08053472770428,
1.28727233489076));
#22847=CARTESIAN_POINT('Ctrl Pts',(-0.00195919018135123,-1.30462473967982,
1.54044292999952));
#22848=CARTESIAN_POINT('Ctrl Pts',(0.154805815536382,-1.45580038421926,
1.74808806061869));
#22849=CARTESIAN_POINT('Ctrl Pts',(0.428137407783241,-1.5340616613226,1.91020772674828));
#22850=CARTESIAN_POINT('Ctrl Pts',(-0.0853753293366669,-1.07622999908393,
1.28727233489076));
#22851=CARTESIAN_POINT('Ctrl Pts',(-0.0542581740029555,-1.30138937207125,
1.54044292999952));
#22852=CARTESIAN_POINT('Ctrl Pts',(0.0960667204863546,-1.45848408198029,
1.74808806061869));
#22853=CARTESIAN_POINT('Ctrl Pts',(0.365599354131263,-1.54751412881105,
1.91020772674828));
#22854=CARTESIAN_POINT('Ctrl Pts',(-0.128593049303377,-1.07192527046357,
1.28727233489076));
#22855=CARTESIAN_POINT('Ctrl Pts',(-0.10655715782456,-1.29815400446268,
1.54044292999952));
#22856=CARTESIAN_POINT('Ctrl Pts',(0.0373276254363271,-1.46116777974132,
1.74808806061869));
#22857=CARTESIAN_POINT('Ctrl Pts',(0.303061300479284,-1.56096659629949,
1.91020772674828));
#22858=CARTESIAN_POINT('Ctrl Pts',(-0.171810769270086,-1.06762054184321,
1.28727233489076));
#22859=CARTESIAN_POINT('Ctrl Pts',(-0.158856141646164,-1.29491863685411,
1.54044292999952));
#22860=CARTESIAN_POINT('Ctrl Pts',(-0.0214114696137,-1.46385147750235,1.74808806061869));
#22861=CARTESIAN_POINT('Ctrl Pts',(0.240523246827306,-1.57441906378793,
1.91020772674828));
#22862=CARTESIAN_POINT('Ctrl Pts',(-0.0421576093699572,-1.08053472770428,
1.28727233489076));
#22863=CARTESIAN_POINT('Ctrl Pts',(-0.0637496973860272,-1.07899219081063,
1.28797191329046));
#22864=CARTESIAN_POINT('Ctrl Pts',(-0.0853207093795707,-1.07715333835806,
1.28831907556383));
#22865=CARTESIAN_POINT('Ctrl Pts',(-0.106872735707655,-1.07501072349525,
1.288319084765));
#22866=CARTESIAN_POINT('Ctrl Pts',(-0.128559621036833,-1.07285470149866,
1.28831909402374));
#22867=CARTESIAN_POINT('Ctrl Pts',(-0.150205375722342,-1.07039324377381,
1.28796761487395));
#22868=CARTESIAN_POINT('Ctrl Pts',(-0.171810769270086,-1.06762054184321,
1.28727233489076));
#22869=CARTESIAN_POINT('Origin',(0.,0.,1.37171309575435));
#22870=CARTESIAN_POINT('',(-0.36490527784414,-1.20742290720348,1.10727038327973));
#22871=CARTESIAN_POINT('Ctrl Pts',(0.0276890267571667,-1.86363850813291,
1.63615580822897));
#22872=CARTESIAN_POINT('Ctrl Pts',(-0.0698239366988097,-1.80655480211407,
1.58477934055792));
#22873=CARTESIAN_POINT('Ctrl Pts',(-0.14869194528843,-1.74187241700968,
1.53343685544663));
#22874=CARTESIAN_POINT('Ctrl Pts',(-0.274785130849248,-1.59669345888594,
1.42076782591243));
#22875=CARTESIAN_POINT('Ctrl Pts',(-0.320436333138567,-1.51444831269989,
1.35830292226021));
#22876=CARTESIAN_POINT('Ctrl Pts',(-0.36627106501613,-1.35321270714143,
1.23020598103186));
#22877=CARTESIAN_POINT('Ctrl Pts',(-0.371649422530895,-1.27957619027631,
1.16961370091491));
#22878=CARTESIAN_POINT('Ctrl Pts',(-0.364905277844141,-1.20742290720348,
1.10727038327973));
#22879=CARTESIAN_POINT('Origin',(0.,0.,1.10727038327973));
#22880=CARTESIAN_POINT('Ctrl Pts',(-0.492368803403902,-0.958722904333223,
1.28318567027397));
#22881=CARTESIAN_POINT('Ctrl Pts',(-0.551909716442827,-1.17966054547972,
1.53751096017971));
#22882=CARTESIAN_POINT('Ctrl Pts',(-0.474301142999538,-1.38346957888851,
1.74607168007007));
#22883=CARTESIAN_POINT('Ctrl Pts',(-0.259543083074032,-1.57015000455958,
1.90886782994505));
#22884=CARTESIAN_POINT('Ctrl Pts',(-0.497730308181424,-0.97247283635693,
1.26847940010162));
#22885=CARTESIAN_POINT('Ctrl Pts',(-0.557797896845799,-1.196516618136,1.51987665322458));
#22886=CARTESIAN_POINT('Ctrl Pts',(-0.478816264707968,-1.40288697684033,
1.72611612827484));
#22887=CARTESIAN_POINT('Ctrl Pts',(-0.260856494176601,-1.59185117960571,
1.88704325648016));
#22888=CARTESIAN_POINT('Ctrl Pts',(-0.510779460904228,-0.996638068239391,
1.24117819097188));
#22889=CARTESIAN_POINT('Ctrl Pts',(-0.572460097309861,-1.22627731830139,
1.48716579746039));
#22890=CARTESIAN_POINT('Ctrl Pts',(-0.491635127338186,-1.43799804358595,
1.68888670640878));
#22891=CARTESIAN_POINT('Ctrl Pts',(-0.268313724592158,-1.63180052564182,
1.84634350908918));
#22892=CARTESIAN_POINT('Ctrl Pts',(-0.557803663431837,-1.04217697649275,
1.18072535874295));
#22893=CARTESIAN_POINT('Ctrl Pts',(-0.62733559714006,-1.28344787385866,
1.41461088358276));
#22894=CARTESIAN_POINT('Ctrl Pts',(-0.546077997260112,-1.50844372983685,
1.60644436926605));
#22895=CARTESIAN_POINT('Ctrl Pts',(-0.314053900652124,-1.71730828939988,
1.75613814413928));
#22896=CARTESIAN_POINT('Ctrl Pts',(-0.608738508149428,-1.07063174084474,
1.13430117558029));
#22897=CARTESIAN_POINT('Ctrl Pts',(-0.687608854742564,-1.32002833380447,
1.35902160674437));
#22898=CARTESIAN_POINT('Ctrl Pts',(-0.608917570976486,-1.55649910176849,
1.54332567193683));
#22899=CARTESIAN_POINT('Ctrl Pts',(-0.372863601758234,-1.78021953810236,
1.68715809360678));
#22900=CARTESIAN_POINT('Ctrl Pts',(-0.649605006049397,-1.08812946536139,
1.10192284729582));
#22901=CARTESIAN_POINT('Ctrl Pts',(-0.736085457637467,-1.34295142581462,
1.32027771712106));
#22902=CARTESIAN_POINT('Ctrl Pts',(-0.660325994321481,-1.58796351671871,
1.49933702411959));
#22903=CARTESIAN_POINT('Ctrl Pts',(-0.422326616101438,-1.82316573807367,
1.63910076829143));
#22904=CARTESIAN_POINT('',(-0.493314642657339,-0.962275025729455,1.28727233489076));
#22905=CARTESIAN_POINT('',(-0.642908916934723,-1.08521613661244,1.10727038327973));
#22906=CARTESIAN_POINT('Ctrl Pts',(-0.493314642657339,-0.962275025729455,
1.28727233489076));
#22907=CARTESIAN_POINT('Ctrl Pts',(-0.505155444616883,-0.992714976574576,
1.25478273943443));
#22908=CARTESIAN_POINT('Ctrl Pts',(-0.522900410114185,-1.0134702004972,
1.22829923781244));
#22909=CARTESIAN_POINT('Ctrl Pts',(-0.572202237708348,-1.05095536138805,
1.17205963503303));
#22910=CARTESIAN_POINT('Ctrl Pts',(-0.603178396561744,-1.06919273067066,
1.14130666672502));
#22911=CARTESIAN_POINT('Ctrl Pts',(-0.642908916934723,-1.08521613661244,
1.10727038327973));
#22912=CARTESIAN_POINT('Ctrl Pts',(-0.493314642657339,-0.962275025729455,
1.28727233489076));
#22913=CARTESIAN_POINT('Ctrl Pts',(-0.519074140629024,-1.06019965524839,
1.39987124007464));
#22914=CARTESIAN_POINT('Ctrl Pts',(-0.517846241724568,-1.15475382712427,
1.50346488650363));
#22915=CARTESIAN_POINT('Ctrl Pts',(-0.454602843714802,-1.35913828497575,
1.715480776583));
#22916=CARTESIAN_POINT('Ctrl Pts',(-0.377981286365637,-1.46714441944577,
1.81902921434248));
#22917=CARTESIAN_POINT('Ctrl Pts',(-0.259766273896474,-1.5699559447672,
1.90869858745619));
#22918=CARTESIAN_POINT('Ctrl Pts',(-0.642908916934723,-1.08521613661244,
1.10727038327973));
#22919=CARTESIAN_POINT('Ctrl Pts',(-0.668710261798003,-1.16760035714813,
1.18103565901042));
#22920=CARTESIAN_POINT('Ctrl Pts',(-0.681355585835302,-1.25518160519556,
1.25302429310885));
#22921=CARTESIAN_POINT('Ctrl Pts',(-0.665371573463992,-1.44098614169382,
1.39260788389873));
#22922=CARTESIAN_POINT('Ctrl Pts',(-0.63530114956013,-1.53389259595497,
1.45574709063856));
#22923=CARTESIAN_POINT('Ctrl Pts',(-0.541698310562567,-1.69239761845938,
1.55895701082587));
#22924=CARTESIAN_POINT('Ctrl Pts',(-0.489122861296312,-1.75616935678546,
1.59904902099409));
#22925=CARTESIAN_POINT('Ctrl Pts',(-0.428377445609995,-1.81394816223928,
1.63615580822897));
#22926=CARTESIAN_POINT('Ctrl Pts',(-0.362330138275325,-1.21487793679796,
1.10149705943222));
#22927=CARTESIAN_POINT('Ctrl Pts',(-0.383459937582896,-1.4832989591636,
1.31979778023781));
#22928=CARTESIAN_POINT('Ctrl Pts',(-0.249644960941924,-1.70227260218964,
1.49880741124996));
#22929=CARTESIAN_POINT('Ctrl Pts',(0.039114791647589,-1.87179886587609,
1.63852595246867));
#22930=CARTESIAN_POINT('Ctrl Pts',(-0.373447482460585,-1.18333690797344,
1.12583385309083));
#22931=CARTESIAN_POINT('Ctrl Pts',(-0.3983051825378,-1.4457367248385,1.34892944774501));
#22932=CARTESIAN_POINT('Ctrl Pts',(-0.270675994878911,-1.66212671668264,
1.5318660237053));
#22933=CARTESIAN_POINT('Ctrl Pts',(0.0093036513012339,-1.83255854794257,
1.67464838892921));
#22934=CARTESIAN_POINT('Ctrl Pts',(-0.386758017000778,-1.13169790455623,
1.16764044916317));
#22935=CARTESIAN_POINT('Ctrl Pts',(-0.416680587119745,-1.38402127269752,
1.39897336709084));
#22936=CARTESIAN_POINT('Ctrl Pts',(-0.298670375694665,-1.59542335194443,
1.58871211231352));
#22937=CARTESIAN_POINT('Ctrl Pts',(-0.0327265383253417,-1.76604232095016,
1.73676275687621));
#22938=CARTESIAN_POINT('Ctrl Pts',(-0.391671741837561,-1.06341115236231,
1.2280160761933));
#22939=CARTESIAN_POINT('Ctrl Pts',(-0.425665904909547,-1.30168216224368,
1.47139032317727));
#22940=CARTESIAN_POINT('Ctrl Pts',(-0.318647566754324,-1.50457544636211,
1.67096220367119));
#22941=CARTESIAN_POINT('Ctrl Pts',(-0.0706042875438574,-1.67209124376878,
1.82672793765153));
#22942=CARTESIAN_POINT('Ctrl Pts',(-0.38218165487343,-1.0286884268729,1.263527751515));
#22943=CARTESIAN_POINT('Ctrl Pts',(-0.415770412604395,-1.25929056133868,
1.51397381108002));
#22944=CARTESIAN_POINT('Ctrl Pts',(-0.312692596804326,-1.45588630034145,
1.71945276482243));
#22945=CARTESIAN_POINT('Ctrl Pts',(-0.0729619965738882,-1.61878272768801,
1.8797604367197));
#22946=CARTESIAN_POINT('Ctrl Pts',(-0.373486051297297,-1.01098164381094,
1.28318517919159));
#22947=CARTESIAN_POINT('Ctrl Pts',(-0.40602648967972,-1.23750736860246,
1.53754499301511));
#22948=CARTESIAN_POINT('Ctrl Pts',(-0.304436793685258,-1.43052436008972,
1.74612783237315));
#22949=CARTESIAN_POINT('Ctrl Pts',(-0.0687169633139101,-1.59003261827273,
1.90893369726572));
#22950=CARTESIAN_POINT('',(-0.373997862975654,-1.01462217612883,1.28727233489076));
#22951=CARTESIAN_POINT('Ctrl Pts',(-0.364905277844141,-1.20742290720348,
1.10727038327973));
#22952=CARTESIAN_POINT('Ctrl Pts',(-0.373615945090689,-1.18311862080926,
1.12801545944052));
#22953=CARTESIAN_POINT('Ctrl Pts',(-0.381365818655258,-1.15609247800023,
1.15133239961429));
#22954=CARTESIAN_POINT('Ctrl Pts',(-0.389206856698301,-1.10715678825424,
1.19509600545515));
#22955=CARTESIAN_POINT('Ctrl Pts',(-0.390682503085324,-1.08733497046169,
1.21324740617476));
#22956=CARTESIAN_POINT('Ctrl Pts',(-0.388091095569743,-1.05408067239125,
1.24538218411121));
#22957=CARTESIAN_POINT('Ctrl Pts',(-0.384447468688947,-1.0359521917548,
1.26364457695037));
#22958=CARTESIAN_POINT('Ctrl Pts',(-0.373997862975654,-1.01462217612883,
1.28727233489076));
#22959=CARTESIAN_POINT('Ctrl Pts',(-0.373997862975654,-1.01462217612883,
1.28727233489076));
#22960=CARTESIAN_POINT('Ctrl Pts',(-0.387792676785359,-1.11493412912611,
1.39987124007464));
#22961=CARTESIAN_POINT('Ctrl Pts',(-0.375201374409042,-1.20865423507634,
1.50346488650363));
#22962=CARTESIAN_POINT('Ctrl Pts',(-0.287835131123856,-1.40394856048621,
1.715480776583));
#22963=CARTESIAN_POINT('Ctrl Pts',(-0.198779555753984,-1.50195515531182,
1.81902921434248));
#22964=CARTESIAN_POINT('Ctrl Pts',(-0.0690572297370888,-1.58980227845634,
1.90869858745619));
#22965=CARTESIAN_POINT('Ctrl Pts',(-0.373997862975653,-1.01462217612883,
1.28727233489076));
#22966=CARTESIAN_POINT('Ctrl Pts',(-0.405014516431691,-1.24016643693111,
1.54044292999952));
#22967=CARTESIAN_POINT('Ctrl Pts',(-0.302637979515068,-1.43238606966553,
1.74808806061869));
#22968=CARTESIAN_POINT('Ctrl Pts',(-0.0668682522257825,-1.59128107433209,
1.91020772674828));
#22969=CARTESIAN_POINT('Ctrl Pts',(-0.413770122869549,-0.997173125995706,
1.28727233489076));
#22970=CARTESIAN_POINT('Ctrl Pts',(-0.453754022216744,-1.22092814469495,
1.54044292999952));
#22971=CARTESIAN_POINT('Ctrl Pts',(-0.359331486839601,-1.41678703930426,
1.74808806061869));
#22972=CARTESIAN_POINT('Ctrl Pts',(-0.130502516738118,-1.58474980982363,
1.91020772674828));
#22973=CARTESIAN_POINT('Ctrl Pts',(-0.453542382763444,-0.979724075862581,
1.28727233489076));
#22974=CARTESIAN_POINT('Ctrl Pts',(-0.502493528001797,-1.2016898524588,
1.54044292999952));
#22975=CARTESIAN_POINT('Ctrl Pts',(-0.416024994164134,-1.40118800894299,
1.74808806061869));
#22976=CARTESIAN_POINT('Ctrl Pts',(-0.194136781250454,-1.57821854531517,
1.91020772674828));
#22977=CARTESIAN_POINT('Ctrl Pts',(-0.493314642657339,-0.962275025729455,
1.28727233489076));
#22978=CARTESIAN_POINT('Ctrl Pts',(-0.55123303378685,-1.18245156022264,
1.54044292999952));
#22979=CARTESIAN_POINT('Ctrl Pts',(-0.472718501488667,-1.38558897858172,
1.74808806061869));
#22980=CARTESIAN_POINT('Ctrl Pts',(-0.257771045762789,-1.5716872808067,
1.91020772674828));
#22981=CARTESIAN_POINT('Ctrl Pts',(-0.373997862975653,-1.01462217612883,
1.28727233489076));
#22982=CARTESIAN_POINT('Ctrl Pts',(-0.394056488869187,-1.00648281422348,
1.28797191329047));
#22983=CARTESIAN_POINT('Ctrl Pts',(-0.414003503730723,-0.998068152324091,
1.28831907556383));
#22984=CARTESIAN_POINT('Ctrl Pts',(-0.433838594404394,-0.989370462098315,
1.288319084765));
#22985=CARTESIAN_POINT('Ctrl Pts',(-0.453797800577657,-0.980618347207412,
1.28831909402374));
#22986=CARTESIAN_POINT('Ctrl Pts',(-0.473623504353515,-0.971588455744714,
1.28796761487395));
#22987=CARTESIAN_POINT('Ctrl Pts',(-0.493314642657339,-0.962275025729455,
1.28727233489076));
#22988=CARTESIAN_POINT('Origin',(0.,0.,1.37171309575435));
#22989=CARTESIAN_POINT('',(-0.720159740047642,-1.03556549162895,1.10727038327973));
#22990=CARTESIAN_POINT('Ctrl Pts',(-0.549562141057369,-1.78098192700405,
1.63615580822897));
#22991=CARTESIAN_POINT('Ctrl Pts',(-0.620893161259053,-1.70079633666903,
1.58735805514616));
#22992=CARTESIAN_POINT('Ctrl Pts',(-0.67413336725818,-1.61925404078178,
1.53858095020846));
#22993=CARTESIAN_POINT('Ctrl Pts',(-0.751969574388241,-1.44461319502364,
1.42806953503217));
#22994=CARTESIAN_POINT('Ctrl Pts',(-0.772017157909609,-1.35007152673693,
1.36461306044574));
#22995=CARTESIAN_POINT('Ctrl Pts',(-0.767479006699504,-1.17779635313151,
1.23357020765533));
#22996=CARTESIAN_POINT('Ctrl Pts',(-0.749676646324456,-1.10397180136273,
1.17136442658357));
#22997=CARTESIAN_POINT('Ctrl Pts',(-0.720159740047643,-1.03556549162895,
1.10727038327973));
#22998=CARTESIAN_POINT('Origin',(0.,0.,1.10727038327973));
#22999=CARTESIAN_POINT('Ctrl Pts',(-0.764532229233201,-0.759649337735664,
1.28318567027397));
#23000=CARTESIAN_POINT('Ctrl Pts',(-0.889432488376416,-0.951374367053292,
1.53751096017971));
#23001=CARTESIAN_POINT('Ctrl Pts',(-0.87860280381325,-1.16919064445971,
1.74607168007007));
#23002=CARTESIAN_POINT('Ctrl Pts',(-0.732043175543704,-1.4130981699549,
1.90886782994505));
#23003=CARTESIAN_POINT('Ctrl Pts',(-0.773880285955837,-0.771069504093749,
1.26847940010162));
#23004=CARTESIAN_POINT('Ctrl Pts',(-0.900241293626992,-0.965585896981723,
1.51987665322458));
#23005=CARTESIAN_POINT('Ctrl Pts',(-0.888897245689575,-1.18626243797171,
1.72611612827484));
#23006=CARTESIAN_POINT('Ctrl Pts',(-0.739998335618538,-1.43333134754249,
1.88704325648016));
#23007=CARTESIAN_POINT('Ctrl Pts',(-0.793756470105422,-0.79001938035927,
1.24117952306876));
#23008=CARTESIAN_POINT('Ctrl Pts',(-0.923380672132909,-0.989358920654668,
1.48716712955727));
#23009=CARTESIAN_POINT('Ctrl Pts',(-0.911936310735738,-1.21569285383181,
1.68888851879237));
#23010=CARTESIAN_POINT('Ctrl Pts',(-0.759433295933266,-1.4690200759214,
1.84634532147277));
#23011=CARTESIAN_POINT('Ctrl Pts',(-0.852549487780078,-0.818798433422952,
1.18072779772815));
#23012=CARTESIAN_POINT('Ctrl Pts',(-0.993235093958044,-1.02677414338758,
1.41461332256795));
#23013=CARTESIAN_POINT('Ctrl Pts',(-0.985480669746803,-1.26586652272338,
1.60644767971085));
#23014=CARTESIAN_POINT('Ctrl Pts',(-0.829355339157893,-1.53620791207527,
1.75614145458407));
#23015=CARTESIAN_POINT('Ctrl Pts',(-0.909788127533563,-0.830120749534188,
1.13430117558028));
#23016=CARTESIAN_POINT('Ctrl Pts',(-1.06186607016719,-1.04293872696083,
1.35902160674436));
#23017=CARTESIAN_POINT('Ctrl Pts',(-1.06009969793961,-1.29215273573923,
1.54332567193682));
#23018=CARTESIAN_POINT('Ctrl Pts',(-0.904732449133398,-1.57786820262105,
1.68715809360678));
#23019=CARTESIAN_POINT('Ctrl Pts',(-0.954061570898026,-0.834133632104406,
1.10192284729582));
#23020=CARTESIAN_POINT('Ctrl Pts',(-1.115053684233,-1.04975978886662,1.32027771712106));
#23021=CARTESIAN_POINT('Ctrl Pts',(-1.11871505289201,-1.30619109614143,
1.49933702411959));
#23022=CARTESIAN_POINT('Ctrl Pts',(-0.965045676875064,-1.60342755392882,
1.63910076829143));
#23023=CARTESIAN_POINT('',(-0.766529441696069,-0.762735325532963,1.28727233489076));
#23024=CARTESIAN_POINT('',(-0.946792943618195,-0.833432097145889,1.10727038327973));
#23025=CARTESIAN_POINT('Ctrl Pts',(-0.766529441696069,-0.762735325532963,
1.28727233489076));
#23026=CARTESIAN_POINT('Ctrl Pts',(-0.787197175677101,-0.788026430107593,
1.25478273943417));
#23027=CARTESIAN_POINT('Ctrl Pts',(-0.810487357658964,-0.80228232516309,
1.22829923781215));
#23028=CARTESIAN_POINT('Ctrl Pts',(-0.868959733810231,-0.822697729112325,
1.17205963503244));
#23029=CARTESIAN_POINT('Ctrl Pts',(-0.904055468578107,-0.83047033850234,
1.14130666672486));
#23030=CARTESIAN_POINT('Ctrl Pts',(-0.946792943618196,-0.833432097145889,
1.10727038327973));
#23031=CARTESIAN_POINT('Ctrl Pts',(-0.766529441696069,-0.762735325532963,
1.28727233489076));
#23032=CARTESIAN_POINT('Ctrl Pts',(-0.821288554787752,-0.847907059902912,
1.39987124007464));
#23033=CARTESIAN_POINT('Ctrl Pts',(-0.849339599532016,-0.938212862837218,
1.50346488650363));
#23034=CARTESIAN_POINT('Ctrl Pts',(-0.852349824604396,-1.15213731807335,
1.715480776583));
#23035=CARTESIAN_POINT('Ctrl Pts',(-0.812854124246773,-1.27853461941729,
1.81902921434248));
#23036=CARTESIAN_POINT('Ctrl Pts',(-0.732195474855993,-1.41284463836769,
1.90869858745619));
#23037=CARTESIAN_POINT('Ctrl Pts',(-0.946792943618196,-0.833432097145889,
1.10727038327973));
#23038=CARTESIAN_POINT('Ctrl Pts',(-0.99678960499347,-0.90381109288579,
1.18103565901043));
#23039=CARTESIAN_POINT('Ctrl Pts',(-1.03588011685504,-0.983198189519685,
1.25302429310889));
#23040=CARTESIAN_POINT('Ctrl Pts',(-1.07809517714267,-1.16484813617463,
1.39260788389878));
#23041=CARTESIAN_POINT('Ctrl Pts',(-1.07820617779495,-1.26249969691992,
1.4557470906386));
#23042=CARTESIAN_POINT('Ctrl Pts',(-1.03816533347022,-1.44217179941021,
1.55895701082589));
#23043=CARTESIAN_POINT('Ctrl Pts',(-1.007869660752,-1.51906903401084,1.5990490209941));
#23044=CARTESIAN_POINT('Ctrl Pts',(-0.967951970128401,-1.59279130921887,
1.63615580822897));
#23045=CARTESIAN_POINT('Ctrl Pts',(-0.720016914634041,-1.04334803864883,
1.10157231096021));
#23046=CARTESIAN_POINT('Ctrl Pts',(-0.823064346331376,-1.29208090893697,
1.31988785480616));
#23047=CARTESIAN_POINT('Ctrl Pts',(-0.763481187915702,-1.54167481933165,
1.4989096332868));
#23048=CARTESIAN_POINT('Ctrl Pts',(-0.541267439387021,-1.79212976983287,
1.63863764640215));
#23049=CARTESIAN_POINT('Ctrl Pts',(-0.720837529677193,-1.00993315330315,
1.12589971949674));
#23050=CARTESIAN_POINT('Ctrl Pts',(-0.825567715093926,-1.25179094217684,
1.34900830339198));
#23051=CARTESIAN_POINT('Ctrl Pts',(-0.771065844731935,-1.49701757504304,
1.53195557707746));
#23052=CARTESIAN_POINT('Ctrl Pts',(-0.557477346013107,-1.74562013410099,
1.6747462494124));
#23053=CARTESIAN_POINT('Ctrl Pts',(-0.717530565095651,-0.956735633325587,
1.16769179538367));
#23054=CARTESIAN_POINT('Ctrl Pts',(-0.823961384252211,-1.18745042322669,
1.39903449435105));
#23055=CARTESIAN_POINT('Ctrl Pts',(-0.777060632929274,-1.42496257773993,
1.58878199846585));
#23056=CARTESIAN_POINT('Ctrl Pts',(-0.576871348730688,-1.66940588754285,
1.73683890344257));
#23057=CARTESIAN_POINT('Ctrl Pts',(-0.701101131459804,-0.890308540641216,
1.22804130170824));
#23058=CARTESIAN_POINT('Ctrl Pts',(-0.807060009317132,-1.10640797973512,
1.47142017171286));
#23059=CARTESIAN_POINT('Ctrl Pts',(-0.767978311363816,-1.33243573819092,
1.67099665961544));
#23060=CARTESIAN_POINT('Ctrl Pts',(-0.583845206097259,-1.56839818009432,
1.82676536339564));
#23061=CARTESIAN_POINT('Ctrl Pts',(-0.681352489183287,-0.86023395370564,
1.2635364344865));
#23062=CARTESIAN_POINT('Ctrl Pts',(-0.784556163294569,-1.06916866744104,
1.51398418220584));
#23063=CARTESIAN_POINT('Ctrl Pts',(-0.747275208483433,-1.28799335847826,
1.71946457116169));
#23064=CARTESIAN_POINT('Ctrl Pts',(-0.569616647707411,-1.51699586639176,
1.87977332297458));
#23065=CARTESIAN_POINT('Ctrl Pts',(-0.667616851769879,-0.846087143187382,
1.28318517919043));
#23066=CARTESIAN_POINT('Ctrl Pts',(-0.768564946360842,-1.05147036139455,
1.53754499301448));
#23067=CARTESIAN_POINT('Ctrl Pts',(-0.731592934569703,-1.26643337142019,
1.74612783237292));
#23068=CARTESIAN_POINT('Ctrl Pts',(-0.556700816396459,-1.4909761732643,
1.90893369726574));
#23069=CARTESIAN_POINT('',(-0.669228599956957,-0.849391336665505,1.28727233489076));
#23070=CARTESIAN_POINT('Ctrl Pts',(-0.720159740047643,-1.03556549162895,
1.10727038327973));
#23071=CARTESIAN_POINT('Ctrl Pts',(-0.720933639361787,-1.00975899746819,
1.12801545944061));
#23072=CARTESIAN_POINT('Ctrl Pts',(-0.719952669695422,-0.981660765603669,
1.15133239961436));
#23073=CARTESIAN_POINT('Ctrl Pts',(-0.712287980257843,-0.932697144982725,
1.19509600545502));
#23074=CARTESIAN_POINT('Ctrl Pts',(-0.707566124812642,-0.913389476194881,
1.21324740617476));
#23075=CARTESIAN_POINT('Ctrl Pts',(-0.694825406568517,-0.882563548281155,
1.24538218411192));
#23076=CARTESIAN_POINT('Ctrl Pts',(-0.685758102881575,-0.866448281268892,
1.26364457695099));
#23077=CARTESIAN_POINT('Ctrl Pts',(-0.669228599956957,-0.849391336665505,
1.28727233489076));
#23078=CARTESIAN_POINT('Ctrl Pts',(-0.669228599956957,-0.849391336665505,
1.28727233489076));
#23079=CARTESIAN_POINT('Ctrl Pts',(-0.713346345736856,-0.940530841324424,
1.39987124007464));
#23080=CARTESIAN_POINT('Ctrl Pts',(-0.73033241101646,-1.03355488521186,
1.50346488650363));
#23081=CARTESIAN_POINT('Ctrl Pts',(-0.707591441492497,-1.2462884798982,
1.715480776583));
#23082=CARTESIAN_POINT('Ctrl Pts',(-0.653180259586498,-1.36701797678012,
1.81902921434248));
#23083=CARTESIAN_POINT('Ctrl Pts',(-0.55695325007777,-1.49065195897357,
1.90869858745619));
#23084=CARTESIAN_POINT('Ctrl Pts',(-0.669228599956957,-0.849391336665505,
1.28727233489076));
#23085=CARTESIAN_POINT('Ctrl Pts',(-0.76842419991163,-1.05431200258793,
1.54044292999952));
#23086=CARTESIAN_POINT('Ctrl Pts',(-0.73045746052879,-1.26875982659235,
1.74808806061869));
#23087=CARTESIAN_POINT('Ctrl Pts',(-0.555328381808437,-1.49273480867877,
1.91020772674828));
#23088=CARTESIAN_POINT('Ctrl Pts',(-0.701662213869994,-0.820505999621324,
1.28727233489076));
#23089=CARTESIAN_POINT('Ctrl Pts',(-0.808833265245786,-1.02095396380933,
1.54044292999952));
#23090=CARTESIAN_POINT('Ctrl Pts',(-0.779555824624011,-1.23640500988538,
1.74808806061869));
#23091=CARTESIAN_POINT('Ctrl Pts',(-0.613829892004671,-1.46685913784949,
1.91020772674828));
#23092=CARTESIAN_POINT('Ctrl Pts',(-0.734095827783032,-0.791620662577143,
1.28727233489076));
#23093=CARTESIAN_POINT('Ctrl Pts',(-0.849242330579942,-0.98759592503072,
1.54044292999952));
#23094=CARTESIAN_POINT('Ctrl Pts',(-0.828654188719232,-1.20405019317841,
1.74808806061869));
#23095=CARTESIAN_POINT('Ctrl Pts',(-0.672331402200905,-1.4409834670202,
1.91020772674828));
#23096=CARTESIAN_POINT('Ctrl Pts',(-0.766529441696069,-0.762735325532963,
1.28727233489076));
#23097=CARTESIAN_POINT('Ctrl Pts',(-0.889651395914097,-0.954237886252114,
1.54044292999952));
#23098=CARTESIAN_POINT('Ctrl Pts',(-0.877752552814453,-1.17169537647143,
1.74808806061869));
#23099=CARTESIAN_POINT('Ctrl Pts',(-0.730832912397138,-1.41510779619092,
1.91020772674828));
#23100=CARTESIAN_POINT('Ctrl Pts',(-0.669228599956957,-0.849391336665505,
1.28727233489076));
#23101=CARTESIAN_POINT('Ctrl Pts',(-0.685790285668801,-0.835451887202035,
1.28797191329047));
#23102=CARTESIAN_POINT('Ctrl Pts',(-0.702160750604673,-0.821285101590929,
1.28831907556383));
#23103=CARTESIAN_POINT('Ctrl Pts',(-0.718337308749603,-0.806883726521851,
1.288319084765));
#23104=CARTESIAN_POINT('Ctrl Pts',(-0.734615089602745,-0.792392236721729,
1.28831909402374));
#23105=CARTESIAN_POINT('Ctrl Pts',(-0.750680064449572,-0.777677820212515,
1.28796761487395));
#23106=CARTESIAN_POINT('Ctrl Pts',(-0.766529441696069,-0.762735325532963,
1.28727233489076));
#23107=CARTESIAN_POINT('Origin',(0.,0.,1.37171309575435));
#23108=CARTESIAN_POINT('',(-1.00491994924733,-0.762339710524744,1.10727038327973));
#23109=CARTESIAN_POINT('Ctrl Pts',(-1.07301833748062,-1.52399042602929,
1.63615580822897));
#23110=CARTESIAN_POINT('Ctrl Pts',(-1.11607945893998,-1.42568690035961,
1.58735805514608));
#23111=CARTESIAN_POINT('Ctrl Pts',(-1.14151594859478,-1.33168344006462,
1.53858095020836));
#23112=CARTESIAN_POINT('Ctrl Pts',(-1.16157559133822,-1.14153741491428,
1.42806953503214));
#23113=CARTESIAN_POINT('Ctrl Pts',(-1.15142699410503,-1.04542790122455,
1.36461306044571));
#23114=CARTESIAN_POINT('Ctrl Pts',(-1.09387499947176,-0.882986840618228,
1.23357020765531));
#23115=CARTESIAN_POINT('Ctrl Pts',(-1.05413090753298,-0.818276751491846,
1.17136442658356));
#23116=CARTESIAN_POINT('Ctrl Pts',(-1.00491994924733,-0.762339710524744,
1.10727038327973));
#23117=CARTESIAN_POINT('Origin',(0.,0.,1.10727038327973));
#23118=CARTESIAN_POINT('Ctrl Pts',(-0.96185791365589,-0.486216001172379,
1.28318567027397));
#23119=CARTESIAN_POINT('Ctrl Pts',(-1.13989141130718,-0.629961036964704,
1.53751096017972));
#23120=CARTESIAN_POINT('Ctrl Pts',(-1.19690070060403,-0.840463183520971,
1.74607168007008));
#23121=CARTESIAN_POINT('Ctrl Pts',(-1.13288578154644,-1.11772244084118,
1.90886782994506));
#23122=CARTESIAN_POINT('Ctrl Pts',(-0.978417321314553,-0.496846021492854,
1.26357731004417));
#23123=CARTESIAN_POINT('Ctrl Pts',(-1.15940183561927,-0.643585521081937,
1.51399891879436));
#23124=CARTESIAN_POINT('Ctrl Pts',(-1.21707904013549,-0.857895946504487,
1.71946418982836));
#23125=CARTESIAN_POINT('Ctrl Pts',(-1.15131005161592,-1.14010192848643,
1.87976839865855));
#23126=CARTESIAN_POINT('Ctrl Pts',(-1.01174306480633,-0.510215828707942,
1.22814964935774));
#23127=CARTESIAN_POINT('Ctrl Pts',(-1.19911435608045,-0.661178469414082,
1.47151698835253));
#23128=CARTESIAN_POINT('Ctrl Pts',(-1.25929534063486,-0.882459067352747,
1.67109028087187));
#23129=CARTESIAN_POINT('Ctrl Pts',(-1.19229498704013,-1.17406335818981,
1.82686350557264));
#23130=CARTESIAN_POINT('Ctrl Pts',(-1.07994419721084,-0.513157287930765,
1.16792318405109));
#23131=CARTESIAN_POINT('Ctrl Pts',(-1.2814248116504,-0.66776628786098,1.39927998114665));
#23132=CARTESIAN_POINT('Ctrl Pts',(-1.35048605385199,-0.899659869879339,
1.58904519906558));
#23133=CARTESIAN_POINT('Ctrl Pts',(-1.28706885932716,-1.20898915642794,
1.73712239616959));
#23134=CARTESIAN_POINT('Ctrl Pts',(-1.1326179950584,-0.505885563397482,
1.12620659350917));
#23135=CARTESIAN_POINT('Ctrl Pts',(-1.34530596753016,-0.661308446532945,
1.34934531900259));
#23136=CARTESIAN_POINT('Ctrl Pts',(-1.42259827975627,-0.900165347523485,
1.53232296148775));
#23137=CARTESIAN_POINT('Ctrl Pts',(-1.3643546712912,-1.22248177762694,1.67514376227794));
#23138=CARTESIAN_POINT('Ctrl Pts',(-1.16512794184932,-0.498486987186291,
1.10192284729582));
#23139=CARTESIAN_POINT('Ctrl Pts',(-1.38487268717996,-0.653810349677837,
1.32027771712106));
#23140=CARTESIAN_POINT('Ctrl Pts',(-1.46759648753937,-0.896559590305325,
1.4993370241196));
#23141=CARTESIAN_POINT('Ctrl Pts',(-1.41329934292755,-1.22673470906876,
1.63910076829144));
#23142=CARTESIAN_POINT('',(-0.964710998256926,-0.488533777383804,1.28727233489076));
#23143=CARTESIAN_POINT('',(-1.15799828028599,-0.500065917147829,1.10727038327973));
#23144=CARTESIAN_POINT('Ctrl Pts',(-0.964710998256926,-0.488533777383804,
1.28727233489076));
#23145=CARTESIAN_POINT('Ctrl Pts',(-0.992182562456595,-0.506200366158372,
1.25478273943432));
#23146=CARTESIAN_POINT('Ctrl Pts',(-1.01873815563829,-0.512561466012044,
1.22829923781232));
#23147=CARTESIAN_POINT('Ctrl Pts',(-1.08065739676493,-0.51390871103861,
1.17205963503494));
#23148=CARTESIAN_POINT('Ctrl Pts',(-1.11643729240226,-0.510455723374939,
1.14130666672712));
#23149=CARTESIAN_POINT('Ctrl Pts',(-1.15799828028599,-0.500065917147829,
1.10727038327973));
#23150=CARTESIAN_POINT('Ctrl Pts',(-0.964710998256926,-0.488533777383804,
1.28727233489076));
#23151=CARTESIAN_POINT('Ctrl Pts',(-1.04310952295002,-0.552615413818275,
1.39987124007464));
#23152=CARTESIAN_POINT('Ctrl Pts',(-1.09769367964031,-0.629833086622262,
1.50346488650363));
#23153=CARTESIAN_POINT('Ctrl Pts',(-1.16666286599128,-0.832357123065218,
1.715480776583));
#23154=CARTESIAN_POINT('Ctrl Pts',(-1.16815913695893,-0.964772942765737,
1.81902921434248));
#23155=CARTESIAN_POINT('Ctrl Pts',(-1.13295228123076,-1.11743425489732,
1.90869858745619));
#23156=CARTESIAN_POINT('Ctrl Pts',(-1.15799828028599,-0.500065917147829,
1.10727038327973));
#23157=CARTESIAN_POINT('Ctrl Pts',(-1.22729623661063,-0.551550501629614,
1.18103565901045));
#23158=CARTESIAN_POINT('Ctrl Pts',(-1.28900548463586,-0.614972484709007,
1.25302429310892));
#23159=CARTESIAN_POINT('Ctrl Pts',(-1.38528731335188,-0.774686679112438,
1.39260788389881));
#23160=CARTESIAN_POINT('Ctrl Pts',(-1.41556887304307,-0.867524531197708,
1.45574709063864));
#23161=CARTESIAN_POINT('Ctrl Pts',(-1.43300950021463,-1.050776156433,1.55895701082591));
#23162=CARTESIAN_POINT('Ctrl Pts',(-1.42795915557246,-1.13327165021093,
1.59904902099411));
#23163=CARTESIAN_POINT('Ctrl Pts',(-1.4127766116927,-1.21572094522251,1.63615580822897));
#23164=CARTESIAN_POINT('Ctrl Pts',(-1.0071890534957,-0.76978548806141,1.1015723109602));
#23165=CARTESIAN_POINT('Ctrl Pts',(-1.18205566887762,-0.974501097544571,
1.31988785480615));
#23166=CARTESIAN_POINT('Ctrl Pts',(-1.2025174778094,-1.230291220982,1.4989096332868));
#23167=CARTESIAN_POINT('Ctrl Pts',(-1.06857448029104,-1.53715585837368,
1.63863764640214));
#23168=CARTESIAN_POINT('Ctrl Pts',(-0.994461965292035,-0.727074783470153,
1.13400885567558));
#23169=CARTESIAN_POINT('Ctrl Pts',(-1.1685858430854,-0.922448816386927,
1.35870212368824));
#23170=CARTESIAN_POINT('Ctrl Pts',(-1.19383871456862,-1.17054629234372,
1.5429783372848));
#23171=CARTESIAN_POINT('Ctrl Pts',(-1.06996683960028,-1.47149928669632,
1.6867824504158));
#23172=CARTESIAN_POINT('Ctrl Pts',(-0.971974682567373,-0.673083751047334,
1.18052322600159));
#23173=CARTESIAN_POINT('Ctrl Pts',(-1.14389365895071,-0.856229621362336,
1.41439979544558));
#23174=CARTESIAN_POINT('Ctrl Pts',(-1.17420151395341,-1.0936426848353,1.60622137130565));
#23175=CARTESIAN_POINT('Ctrl Pts',(-1.06281232835789,-1.38546708108516,
1.75589800730001));
#23176=CARTESIAN_POINT('Ctrl Pts',(-0.932030917609334,-0.621030952892817,
1.24109849008297));
#23177=CARTESIAN_POINT('Ctrl Pts',(-1.09790581924279,-0.791463701885435,
1.48710325590113));
#23178=CARTESIAN_POINT('Ctrl Pts',(-1.13059499103696,-1.01576709402367,
1.6888327560127));
#23179=CARTESIAN_POINT('Ctrl Pts',(-1.03008879377588,-1.29394102274663,
1.84628852230556));
#23180=CARTESIAN_POINT('Ctrl Pts',(-0.909472892481624,-0.605279141158067,
1.26844862066248));
#23181=CARTESIAN_POINT('Ctrl Pts',(-1.07134082867159,-0.771469550259548,
1.51987386218776));
#23182=CARTESIAN_POINT('Ctrl Pts',(-1.10338745862407,-0.990137606500526,
1.72613059618619));
#23183=CARTESIAN_POINT('Ctrl Pts',(-1.00543407447983,-1.26153883267189,
1.88706341654737));
#23184=CARTESIAN_POINT('Ctrl Pts',(-0.89639666323125,-0.598371737953918,
1.28318517919043));
#23185=CARTESIAN_POINT('Ctrl Pts',(-1.055870911185,-0.762508109189138,1.53754499301448));
#23186=CARTESIAN_POINT('Ctrl Pts',(-1.08713566171041,-0.978375060596136,
1.74612783237291));
#23187=CARTESIAN_POINT('Ctrl Pts',(-0.990190914807483,-1.24597259217491,
1.90893369726573));
#23188=CARTESIAN_POINT('',(-0.89895057878464,-0.601016155111926,1.28727233489076));
#23189=CARTESIAN_POINT('Ctrl Pts',(-1.00491994924733,-0.762339710524744,
1.10727038327973));
#23190=CARTESIAN_POINT('Ctrl Pts',(-0.997681325972045,-0.737557128050268,
1.12801545944073));
#23191=CARTESIAN_POINT('Ctrl Pts',(-0.98806553722046,-0.711137257836932,
1.15133239961458));
#23192=CARTESIAN_POINT('Ctrl Pts',(-0.965645393507087,-0.666938606676028,
1.19509600545601));
#23193=CARTESIAN_POINT('Ctrl Pts',(-0.955188244339595,-0.650035056038689,
1.2132474061757));
#23194=CARTESIAN_POINT('Ctrl Pts',(-0.933545365639423,-0.624654954884534,
1.24538218411151));
#23195=CARTESIAN_POINT('Ctrl Pts',(-0.9199419560071,-0.612130376112957,
1.26364457695062));
#23196=CARTESIAN_POINT('Ctrl Pts',(-0.89895057878464,-0.601016155111926,
1.28727233489076));
#23197=CARTESIAN_POINT('Ctrl Pts',(-0.89895057878464,-0.601016155111926,
1.28727233489076));
#23198=CARTESIAN_POINT('Ctrl Pts',(-0.969072704191387,-0.674061841710201,
1.39987124007464));
#23199=CARTESIAN_POINT('Ctrl Pts',(-1.01397342270847,-0.757283981982513,
1.50346488650363));
#23200=CARTESIAN_POINT('Ctrl Pts',(-1.05808377148838,-0.966632999495317,
1.715480776583));
#23201=CARTESIAN_POINT('Ctrl Pts',(-1.04364312863621,-1.09826755410688,
1.81902921434248));
#23202=CARTESIAN_POINT('Ctrl Pts',(-0.990330805779366,-1.24558623976355,
1.90869858745619));
#23203=CARTESIAN_POINT('Ctrl Pts',(-0.89895057878464,-0.601016155111926,
1.28727233489076));
#23204=CARTESIAN_POINT('Ctrl Pts',(-1.056615168778,-0.765254163607779,1.54044292999952));
#23205=CARTESIAN_POINT('Ctrl Pts',(-1.08677467590956,-0.980938531722802,
1.74808806061869));
#23206=CARTESIAN_POINT('Ctrl Pts',(-0.989429100179333,-1.24806925945699,
1.91020772674828));
#23207=CARTESIAN_POINT('Ctrl Pts',(-0.920870718608735,-0.563522029202552,
1.28727233489076));
#23208=CARTESIAN_POINT('Ctrl Pts',(-1.08473827279984,-0.721041695541498,
1.54044292999951));
#23209=CARTESIAN_POINT('Ctrl Pts',(-1.12347180680942,-0.934995043558669,
1.74808806061869));
#23210=CARTESIAN_POINT('Ctrl Pts',(-1.03707132063747,-1.20538207325406,
1.91020772674828));
#23211=CARTESIAN_POINT('Ctrl Pts',(-0.94279085843283,-0.526027903293178,
1.28727233489076));
#23212=CARTESIAN_POINT('Ctrl Pts',(-1.11286137682168,-0.676829227475217,
1.54044292999952));
#23213=CARTESIAN_POINT('Ctrl Pts',(-1.16016893770927,-0.889051555394535,
1.74808806061869));
#23214=CARTESIAN_POINT('Ctrl Pts',(-1.0847135410956,-1.16269488705113,1.91020772674828));
#23215=CARTESIAN_POINT('Ctrl Pts',(-0.964710998256926,-0.488533777383804,
1.28727233489076));
#23216=CARTESIAN_POINT('Ctrl Pts',(-1.14098448084351,-0.632616759408936,
1.54044292999952));
#23217=CARTESIAN_POINT('Ctrl Pts',(-1.19686606860912,-0.843108067230401,
1.74808806061869));
#23218=CARTESIAN_POINT('Ctrl Pts',(-1.13235576155374,-1.1200077008482,1.91020772674828));
#23219=CARTESIAN_POINT('Ctrl Pts',(-0.89895057878464,-0.601016155111926,
1.28727233489076));
#23220=CARTESIAN_POINT('Ctrl Pts',(-0.910394151125288,-0.582641108525654,
1.28797191329047));
#23221=CARTESIAN_POINT('Ctrl Pts',(-0.921585610967828,-0.564108942884259,
1.28831907556383));
#23222=CARTESIAN_POINT('Ctrl Pts',(-0.932520162364073,-0.545413589903933,
1.288319084765));
#23223=CARTESIAN_POINT('Ctrl Pts',(-0.94352313529324,-0.526601253184352,
1.28831909402374));
#23224=CARTESIAN_POINT('Ctrl Pts',(-0.954254829541783,-0.507642661237889,
1.28796761487395));
#23225=CARTESIAN_POINT('Ctrl Pts',(-0.964710998256926,-0.488533777383804,
1.28727233489076));
#23226=CARTESIAN_POINT('Origin',(0.,0.,1.37171309575435));
#23227=CARTESIAN_POINT('',(-1.19131159212569,-0.414490807021284,1.10727038327973));
#23228=CARTESIAN_POINT('Ctrl Pts',(-1.4914400228729,-1.11782012388912,1.63615580822897));
#23229=CARTESIAN_POINT('Ctrl Pts',(-1.50201612299691,-1.01102129689832,
1.58735805514605));
#23230=CARTESIAN_POINT('Ctrl Pts',(-1.49715899547356,-0.913758385849903,
1.53858095020832));
#23231=CARTESIAN_POINT('Ctrl Pts',(-1.45747849623496,-0.726719999074295,
1.42806953503212));
#23232=CARTESIAN_POINT('Ctrl Pts',(-1.41812713365384,-0.638450508815843,
1.3646130604457));
#23233=CARTESIAN_POINT('Ctrl Pts',(-1.31319488582045,-0.501744424014171,
1.23357020765531));
#23234=CARTESIAN_POINT('Ctrl Pts',(-1.25539949095026,-0.452483071915572,
1.17136442658356));
#23235=CARTESIAN_POINT('Ctrl Pts',(-1.19131159212569,-0.414490807021284,
1.10727038327973));
#23236=CARTESIAN_POINT('Origin',(0.,0.,1.10727038327973));
#23237=CARTESIAN_POINT('Ctrl Pts',(-1.06503024383179,-0.165188454748262,
1.28318567027397));
#23238=CARTESIAN_POINT('Ctrl Pts',(-1.27876982080873,-0.246882731381368,
1.53751096017971));
#23239=CARTESIAN_POINT('Ctrl Pts',(-1.39803761752214,-0.429465330327849,
1.74607168007007));
#23240=CARTESIAN_POINT('Ctrl Pts',(-1.42283363397203,-0.712936251587706,
1.90886782994504));
#23241=CARTESIAN_POINT('Ctrl Pts',(-1.07930558594879,-0.168932913531384,
1.26847940010162));
#23242=CARTESIAN_POINT('Ctrl Pts',(-1.29586765564978,-0.252026844288348,
1.51987665322458));
#23243=CARTESIAN_POINT('Ctrl Pts',(-1.41640054440423,-0.437225780288037,
1.72611612827483));
#23244=CARTESIAN_POINT('Ctrl Pts',(-1.44116225705855,-0.72462931033466,
1.88704325648016));
#23245=CARTESIAN_POINT('Ctrl Pts',(-1.10652474870095,-0.172580460092752,
1.24117906537517));
#23246=CARTESIAN_POINT('Ctrl Pts',(-1.32856177300787,-0.25765834155068,
1.48716667186367));
#23247=CARTESIAN_POINT('Ctrl Pts',(-1.45233913898615,-0.447493258920474,
1.68888789608759));
#23248=CARTESIAN_POINT('Ctrl Pts',(-1.47786361346602,-0.742078309759777,
1.84634469876799));
#23249=CARTESIAN_POINT('Ctrl Pts',(-1.171005693206,-0.161305070542798,1.18072695962337));
#23250=CARTESIAN_POINT('Ctrl Pts',(-1.40706779462018,-0.246868029800143,
1.41461248446317));
#23251=CARTESIAN_POINT('Ctrl Pts',(-1.5413299739097,-0.444855864337685,
1.60644654213682));
#23252=CARTESIAN_POINT('Ctrl Pts',(-1.57392460995617,-0.755334809435743,
1.75614031701005));
#23253=CARTESIAN_POINT('Ctrl Pts',(-1.22396679065339,-0.136821749681419,
1.13430117558029));
#23254=CARTESIAN_POINT('Ctrl Pts',(-1.47209169926766,-0.219605938249046,
1.35902160674436));
#23255=CARTESIAN_POINT('Ctrl Pts',(-1.61714699314177,-0.422262554132505,
1.54332567193681));
#23256=CARTESIAN_POINT('Ctrl Pts',(-1.65939158627326,-0.744733799933205,
1.68715809360676));
#23257=CARTESIAN_POINT('Ctrl Pts',(-1.26214347192869,-0.114044962799315,
1.10192284729582));
#23258=CARTESIAN_POINT('Ctrl Pts',(-1.51913070253035,-0.193861398098009,
1.32027771712105));
#23259=CARTESIAN_POINT('Ctrl Pts',(-1.67281935264037,-0.399166585072132,
1.49933702411959));
#23260=CARTESIAN_POINT('Ctrl Pts',(-1.72320942225875,-0.729960523721685,
1.63910076829142));
#23261=CARTESIAN_POINT('',(-1.06845992077163,-0.166511139289342,1.28727233489076));
#23262=CARTESIAN_POINT('',(-1.25585067703094,-0.117749801015222,1.10727038327973));
#23263=CARTESIAN_POINT('Ctrl Pts',(-1.06845992077163,-0.166511139289342,
1.28727233489076));
#23264=CARTESIAN_POINT('Ctrl Pts',(-1.10004620708042,-0.174823883464314,
1.25478273943443));
#23265=CARTESIAN_POINT('Ctrl Pts',(-1.12726776497764,-0.172667519342168,
1.22829923781242));
#23266=CARTESIAN_POINT('Ctrl Pts',(-1.1865727843456,-0.154814727716306,
1.17205963503352));
#23267=CARTESIAN_POINT('Ctrl Pts',(-1.21953445537447,-0.140474145488659,
1.14130666672565));
#23268=CARTESIAN_POINT('Ctrl Pts',(-1.25585067703094,-0.117749801015222,
1.10727038327973));
#23269=CARTESIAN_POINT('Ctrl Pts',(-1.06845992077163,-0.166511139289342,
1.28727233489076));
#23270=CARTESIAN_POINT('Ctrl Pts',(-1.16282366323453,-0.203229920731113,
1.39987124007464));
#23271=CARTESIAN_POINT('Ctrl Pts',(-1.23859785430383,-0.259800859583567,
1.50346488650363));
#23272=CARTESIAN_POINT('Ctrl Pts',(-1.36677481743678,-0.431100013478375,
1.715480776583));
#23273=CARTESIAN_POINT('Ctrl Pts',(-1.40911659430226,-0.556572568507924,
1.81902921434248));
#23274=CARTESIAN_POINT('Ctrl Pts',(-1.42280782457595,-0.712641620935351,
1.90869858745619));
#23275=CARTESIAN_POINT('Ctrl Pts',(-1.25585067703094,-0.117749801015222,
1.10727038327973));
#23276=CARTESIAN_POINT('Ctrl Pts',(-1.33766656151263,-0.145300304395601,
1.18103565901045));
#23277=CARTESIAN_POINT('Ctrl Pts',(-1.41595401455119,-0.186548988329719,
1.25302429310891));
#23278=CARTESIAN_POINT('Ctrl Pts',(-1.55687787546593,-0.308693492339175,
1.3926078838988));
#23279=CARTESIAN_POINT('Ctrl Pts',(-1.61436582414943,-0.387630019962956,
1.45574709063863));
#23280=CARTESIAN_POINT('Ctrl Pts',(-1.68758071271377,-0.556523222076088,
1.5589570108259));
#23281=CARTESIAN_POINT('Ctrl Pts',(-1.70827005906903,-0.63654174132047,
1.59904902099411));
#23282=CARTESIAN_POINT('Ctrl Pts',(-1.71930883511106,-0.71964734468187,
1.63615580822897));
#23283=CARTESIAN_POINT('Ctrl Pts',(-1.19577051030242,-0.420870970491663,
1.1015723109602));
#23284=CARTESIAN_POINT('Ctrl Pts',(-1.425339146688,-0.561530328976118,1.31988785480615));
#23285=CARTESIAN_POINT('Ctrl Pts',(-1.52384297854319,-0.798478145979653,
1.4989096332868));
#23286=CARTESIAN_POINT('Ctrl Pts',(-1.49128200586798,-1.13171442150227,
1.63863764640214));
#23287=CARTESIAN_POINT('Ctrl Pts',(-1.17679362500493,-0.393355414961737,
1.12589971949673));
#23288=CARTESIAN_POINT('Ctrl Pts',(-1.40368256628313,-0.527463617924696,
1.34900830339198));
#23289=CARTESIAN_POINT('Ctrl Pts',(-1.50373022520315,-0.757891527007919,
1.53195557707745));
#23290=CARTESIAN_POINT('Ctrl Pts',(-1.47705841783301,-1.08455939173712,
1.67474624941239));
#23291=CARTESIAN_POINT('Ctrl Pts',(-1.14284817765566,-0.352262141476105,
1.16769296545954));
#23292=CARTESIAN_POINT('Ctrl Pts',(-1.3645632700682,-0.476355861470114,
1.39903566442693));
#23293=CARTESIAN_POINT('Ctrl Pts',(-1.46622517664402,-0.696074558068199,
1.588783597768));
#23294=CARTESIAN_POINT('Ctrl Pts',(-1.44794881615931,-1.01150165877894,
1.73684050274471));
#23295=CARTESIAN_POINT('Ctrl Pts',(-1.09051150146367,-0.308178085105591,
1.22804267083047));
#23296=CARTESIAN_POINT('Ctrl Pts',(-1.30325409768322,-0.42072513805346,
1.47142154083509));
#23297=CARTESIAN_POINT('Ctrl Pts',(-1.40449154295596,-0.626556636662154,
1.6709985296405));
#23298=CARTESIAN_POINT('Ctrl Pts',(-1.39421997501402,-0.925684985930717,
1.82676723342071));
#23299=CARTESIAN_POINT('Ctrl Pts',(-1.05685857441837,-0.295454942931511,
1.2635364344865));
#23300=CARTESIAN_POINT('Ctrl Pts',(-1.26316084408196,-0.403825079433306,
1.51398418220584));
#23301=CARTESIAN_POINT('Ctrl Pts',(-1.36162184430235,-0.602771168700631,
1.71946457116169));
#23302=CARTESIAN_POINT('Ctrl Pts',(-1.35249734632791,-0.892463171324795,
1.87977332297459));
#23303=CARTESIAN_POINT('Ctrl Pts',(-1.03743092373275,-0.292083537908477,
1.28318517919043));
#23304=CARTESIAN_POINT('Ctrl Pts',(-1.23982087453715,-0.398906250549902,
1.53754499301448));
#23305=CARTESIAN_POINT('Ctrl Pts',(-1.33626197576336,-0.594546582101055,
1.74612783237292));
#23306=CARTESIAN_POINT('Ctrl Pts',(-1.32675422741137,-0.879004532561935,
1.90893369726574));
#23307=CARTESIAN_POINT('',(-1.04067701160391,-0.293809324770207,1.28727233489076));
#23308=CARTESIAN_POINT('Ctrl Pts',(-1.19131159212569,-0.414490807021284,
1.10727038327973));
#23309=CARTESIAN_POINT('Ctrl Pts',(-1.1767690131419,-0.393158028076673,
1.12801545944032));
#23310=CARTESIAN_POINT('Ctrl Pts',(-1.1594596657054,-0.371002680489135,
1.15133239961409));
#23311=CARTESIAN_POINT('Ctrl Pts',(-1.12447870759388,-0.335895470715412,
1.19509600545484));
#23312=CARTESIAN_POINT('Ctrl Pts',(-1.10930988332438,-0.323050675538543,
1.21324740617428));
#23313=CARTESIAN_POINT('Ctrl Pts',(-1.08088339992866,-0.305600782276628,
1.24538218411116));
#23314=CARTESIAN_POINT('Ctrl Pts',(-1.06407548086623,-0.297892884779764,
1.26364457695028));
#23315=CARTESIAN_POINT('Ctrl Pts',(-1.04067701160391,-0.293809324770207,
1.28727233489076));
#23316=CARTESIAN_POINT('Ctrl Pts',(-1.04067701160391,-0.293809324770207,
1.28727233489076));
#23317=CARTESIAN_POINT('Ctrl Pts',(-1.12993947443311,-0.341610972564374,
1.39987124007464));
#23318=CARTESIAN_POINT('Ctrl Pts',(-1.19835965101752,-0.406884846288962,
1.50346488650363));
#23319=CARTESIAN_POINT('Ctrl Pts',(-1.30500348982786,-0.592356746173702,
1.715480776583));
#23320=CARTESIAN_POINT('Ctrl Pts',(-1.33194693676576,-0.722011051157661,
1.81902921434248));
#23321=CARTESIAN_POINT('Ctrl Pts',(-1.32676788217082,-0.878593860895847,
1.90869858745619));
#23322=CARTESIAN_POINT('Ctrl Pts',(-1.04067701160391,-0.293809324770207,
1.28727233489076));
#23323=CARTESIAN_POINT('Ctrl Pts',(-1.24137728305361,-0.40128791525442,
1.54044292999952));
#23324=CARTESIAN_POINT('Ctrl Pts',(-1.3367108140079,-0.59709613876759,1.74808806061869));
#23325=CARTESIAN_POINT('Ctrl Pts',(-1.32667760446677,-0.881233995309716,
1.91020772674828));
#23326=CARTESIAN_POINT('Ctrl Pts',(-1.04993798132648,-0.251376596276585,
1.28727233489076));
#23327=CARTESIAN_POINT('Ctrl Pts',(-1.25446154039629,-0.35054884232117,
1.54044292999951));
#23328=CARTESIAN_POINT('Ctrl Pts',(-1.35741454085596,-0.542061247874906,
1.74808806061869));
#23329=CARTESIAN_POINT('Ctrl Pts',(-1.3587969827055,-0.825913812937791,
1.91020772674828));
#23330=CARTESIAN_POINT('Ctrl Pts',(-1.05919895104906,-0.208943867782964,
1.28727233489076));
#23331=CARTESIAN_POINT('Ctrl Pts',(-1.26754579773896,-0.29980976938792,
1.54044292999952));
#23332=CARTESIAN_POINT('Ctrl Pts',(-1.37811826770402,-0.487026356982221,
1.74808806061869));
#23333=CARTESIAN_POINT('Ctrl Pts',(-1.39091636094422,-0.770593630565867,
1.91020772674828));
#23334=CARTESIAN_POINT('Ctrl Pts',(-1.06845992077163,-0.166511139289342,
1.28727233489076));
#23335=CARTESIAN_POINT('Ctrl Pts',(-1.28063005508163,-0.24907069645467,
1.54044292999952));
#23336=CARTESIAN_POINT('Ctrl Pts',(-1.39882199455207,-0.431991466089537,
1.74808806061869));
#23337=CARTESIAN_POINT('Ctrl Pts',(-1.42303573918295,-0.715273448193942,
1.91020772674828));
#23338=CARTESIAN_POINT('Ctrl Pts',(-1.04067701160391,-0.293809324770207,
1.28727233489076));
#23339=CARTESIAN_POINT('Ctrl Pts',(-1.04588229398058,-0.272797358647497,
1.28797191329047));
#23340=CARTESIAN_POINT('Ctrl Pts',(-1.05079925066492,-0.251713870469972,
1.28831907556383));
#23341=CARTESIAN_POINT('Ctrl Pts',(-1.05542144523633,-0.230554570986284,
1.288319084765));
#23342=CARTESIAN_POINT('Ctrl Pts',(-1.06007256258898,-0.209262869938621,
1.28831909402374));
#23343=CARTESIAN_POINT('Ctrl Pts',(-1.06442048323407,-0.187915901626914,
1.28796761487395));
#23344=CARTESIAN_POINT('Ctrl Pts',(-1.06845992077163,-0.166511139289342,
1.28727233489076));
#23345=CARTESIAN_POINT('Origin',(0.,0.,1.37171309575435));
#23346=CARTESIAN_POINT('',(-1.26108935601086,-0.0260686553993158,1.10727038327973));
#23347=CARTESIAN_POINT('Ctrl Pts',(-1.76386916735272,-0.602229799711917,
1.63615580822897));
#23348=CARTESIAN_POINT('Ctrl Pts',(-1.74092498377312,-0.497389884696873,
1.58735805514594));
#23349=CARTESIAN_POINT('Ctrl Pts',(-1.70624968855518,-0.406388294299067,
1.53858095020821));
#23350=CARTESIAN_POINT('Ctrl Pts',(-1.61071325107042,-0.240766166368963,
1.42806953503212));
#23351=CARTESIAN_POINT('Ctrl Pts',(-1.54601110868788,-0.16897713225799,
1.3646130604457));
#23352=CARTESIAN_POINT('Ctrl Pts',(-1.40397010717825,-0.0713877673286483,
1.23357020765531));
#23353=CARTESIAN_POINT('Ctrl Pts',(-1.33378082531076,-0.0423971966252641,
1.17136442658356));
#23354=CARTESIAN_POINT('Ctrl Pts',(-1.26108935601086,-0.0260686553993154,
1.10727038327973));
#23355=CARTESIAN_POINT('Origin',(0.,0.,1.10727038327973));
#23356=CARTESIAN_POINT('Ctrl Pts',(-1.06394999323939,0.172008888562255,
1.28318567027397));
#23357=CARTESIAN_POINT('Ctrl Pts',(-1.2924681694826,0.160362439116273,1.53750521640541));
#23358=CARTESIAN_POINT('Ctrl Pts',(-1.46231719972918,0.023577760251311,
1.74606225962531));
#23359=CARTESIAN_POINT('Ctrl Pts',(-1.57349708397913,-0.23834514803263,
1.90885679993368));
#23360=CARTESIAN_POINT('Ctrl Pts',(-1.07868665224636,0.172859187306825,
1.2684765050474));
#23361=CARTESIAN_POINT('Ctrl Pts',(-1.31032224774096,0.160753683145647,
1.51986749395221));
#23362=CARTESIAN_POINT('Ctrl Pts',(-1.48218332835239,0.0218713714335428,
1.72610289246663));
#23363=CARTESIAN_POINT('Ctrl Pts',(-1.59454606057878,-0.243802874063091,
1.88702805548521));
#23364=CARTESIAN_POINT('Ctrl Pts',(-1.10570688269945,0.177804687773572,
1.24116976953013));
#23365=CARTESIAN_POINT('Ctrl Pts',(-1.34316347164223,0.16550438356704,1.48715026946299));
#23366=CARTESIAN_POINT('Ctrl Pts',(-1.51954478212276,0.0232152493262158,
1.6888660924649));
#23367=CARTESIAN_POINT('Ctrl Pts',(-1.63485294054343,-0.249054092840228,
1.8463203415307));
#23368=CARTESIAN_POINT('Ctrl Pts',(-1.16355954955659,0.208466906889382,
1.18070453025514));
#23369=CARTESIAN_POINT('Ctrl Pts',(-1.41450709648088,0.200040954183215,
1.41458088343679));
#23370=CARTESIAN_POINT('Ctrl Pts',(-1.60338349810865,0.0532384711777712,
1.60640735029516));
#23371=CARTESIAN_POINT('Ctrl Pts',(-1.73033051533549,-0.231963472934464,
1.75609715466375));
#23372=CARTESIAN_POINT('Ctrl Pts',(-1.20636749722078,0.248125754775118,
1.13427327868627));
#23373=CARTESIAN_POINT('Ctrl Pts',(-1.46793051395096,0.246072078233562,
1.35898312394782));
#23374=CARTESIAN_POINT('Ctrl Pts',(-1.66851465914541,0.0981648464084902,
1.54327941073122));
#23375=CARTESIAN_POINT('Ctrl Pts',(-1.80834818125255,-0.195461051586317,
1.68710688538769));
#23376=CARTESIAN_POINT('Ctrl Pts',(-1.235641855012,0.281595159362692,1.10188938448118));
#23377=CARTESIAN_POINT('Ctrl Pts',(-1.50471757474417,0.285104353628414,
1.32023273220194));
#23378=CARTESIAN_POINT('Ctrl Pts',(-1.71433282083683,0.137346783688562,
1.49928348142626));
#23379=CARTESIAN_POINT('Ctrl Pts',(-1.86448759328998,-0.161677550456861,
1.63904163215416));
#23380=CARTESIAN_POINT('',(-1.06762054184321,0.171810769270086,1.28727233489076));
#23381=CARTESIAN_POINT('',(-1.23077165948193,0.27609248605186,1.10727038327973));
#23382=CARTESIAN_POINT('Ctrl Pts',(-1.06762054184321,0.171810769270086,
1.28727233489076));
#23383=CARTESIAN_POINT('Ctrl Pts',(-1.10022966448203,0.173665579012753,
1.25478273943509));
#23384=CARTESIAN_POINT('Ctrl Pts',(-1.12545255134418,0.184128327165882,
1.22829923781306));
#23385=CARTESIAN_POINT('Ctrl Pts',(-1.17633816045214,0.219433599811068,
1.17205963503584));
#23386=CARTESIAN_POINT('Ctrl Pts',(-1.20325508885488,0.243258020496417,
1.14130666672783));
#23387=CARTESIAN_POINT('Ctrl Pts',(-1.23077165948193,0.27609248605186,1.10727038327973));
#23388=CARTESIAN_POINT('Ctrl Pts',(-1.06762054184321,0.171810769270086,
1.28727233489076));
#23389=CARTESIAN_POINT('Ctrl Pts',(-1.16871252149279,0.166049132983329,
1.39987124007464));
#23390=CARTESIAN_POINT('Ctrl Pts',(-1.2582594411694,0.135662485730195,1.50346488650363));
#23391=CARTESIAN_POINT('Ctrl Pts',(-1.43309732687145,0.0123561690781441,
1.715480776583));
#23392=CARTESIAN_POINT('Ctrl Pts',(-1.51213990150266,-0.0938909933754469,
1.81902921434248));
#23393=CARTESIAN_POINT('Ctrl Pts',(-1.57338902476662,-0.238090659850087,
1.90869858745619));
#23394=CARTESIAN_POINT('Ctrl Pts',(-1.23077165948193,0.27609248605186,1.10727038327973));
#23395=CARTESIAN_POINT('Ctrl Pts',(-1.31709676330278,0.275172898999399,
1.18103565901041));
#23396=CARTESIAN_POINT('Ctrl Pts',(-1.40429909999044,0.260135222790514,
1.25302429310884));
#23397=CARTESIAN_POINT('Ctrl Pts',(-1.57122974978687,0.189563202796485,
1.38867432147861));
#23398=CARTESIAN_POINT('Ctrl Pts',(-1.64657149028472,0.13638820421775,1.44891114041812));
#23399=CARTESIAN_POINT('Ctrl Pts',(-1.77077010917836,0.0017905112135637,
1.55340617058598));
#23400=CARTESIAN_POINT('Ctrl Pts',(-1.81883456875388,-0.0722162251277585,
1.59645518670946));
#23401=CARTESIAN_POINT('Ctrl Pts',(-1.85754313061971,-0.153129647965885,
1.63615580822897));
#23402=CARTESIAN_POINT('Ctrl Pts',(-1.26730161813771,-0.030758669949715,
1.1015723109602));
#23403=CARTESIAN_POINT('Ctrl Pts',(-1.52910049789878,-0.0935930593956264,
1.31988785480615));
#23404=CARTESIAN_POINT('Ctrl Pts',(-1.69600411129884,-0.28850446672445,
1.49890963328679));
#23405=CARTESIAN_POINT('Ctrl Pts',(-1.76801245833787,-0.615492891936185,
1.63863764640214));
#23406=CARTESIAN_POINT('Ctrl Pts',(-1.24075075344812,-0.0104540016207254,
1.12589971949672));
#23407=CARTESIAN_POINT('Ctrl Pts',(-1.49797667332671,-0.0678859432465771,
1.34900830339197));
#23408=CARTESIAN_POINT('Ctrl Pts',(-1.66433379116767,-0.256119480862738,
1.53195557707745));
#23409=CARTESIAN_POINT('Ctrl Pts',(-1.73991331668443,-0.575041124025744,
1.67474624941239));
#23410=CARTESIAN_POINT('Ctrl Pts',(-1.19576910668284,0.0181391694102173,
1.16769197379075));
#23411=CARTESIAN_POINT('Ctrl Pts',(-1.44497975845612,-0.0313672401565084,
1.39903467275814));
#23412=CARTESIAN_POINT('Ctrl Pts',(-1.60956344041244,-0.208916886053931,
1.58878224232));
#23413=CARTESIAN_POINT('Ctrl Pts',(-1.68965392328535,-0.514553591586066,
1.73683914729671));
#23414=CARTESIAN_POINT('Ctrl Pts',(-1.13237144427268,0.0438923944102214,
1.22804151155252));
#23415=CARTESIAN_POINT('Ctrl Pts',(-1.36948062872854,0.00259486397362416,
1.47142038155714));
#23416=CARTESIAN_POINT('Ctrl Pts',(-1.52936917527703,-0.161878639424908,
1.67099694623232));
#23417=CARTESIAN_POINT('Ctrl Pts',(-1.61203607707659,-0.449540694258328,
1.82676565001253));
#23418=CARTESIAN_POINT('Ctrl Pts',(-1.09643283244092,0.045592911399531,
1.2635364344865));
#23419=CARTESIAN_POINT('Ctrl Pts',(-1.32612616419274,0.00627769421187267,
1.51398418220585));
#23420=CARTESIAN_POINT('Ctrl Pts',(-1.48124586260133,-0.152505158025998,
1.71946457116169));
#23421=CARTESIAN_POINT('Ctrl Pts',(-1.56208770129018,-0.43083824977955,
1.87977332297459));
#23422=CARTESIAN_POINT('Ctrl Pts',(-1.07691421721301,0.0427958338931189,
1.28318517919043));
#23423=CARTESIAN_POINT('Ctrl Pts',(-1.30240853234962,0.00374333123643575,
1.53754499301448));
#23424=CARTESIAN_POINT('Ctrl Pts',(-1.45458565734394,-0.152519741700302,
1.74612783237292));
#23425=CARTESIAN_POINT('Ctrl Pts',(-1.53344559219597,-0.425993384917094,
1.90893369726574));
#23426=CARTESIAN_POINT('',(-1.22409607597286,-1.56082004234302E-11,1.14453307412866));
#23427=CARTESIAN_POINT('Ctrl Pts',(-1.26108935601086,-0.0260686553993156,
1.10727038327973));
#23428=CARTESIAN_POINT('Ctrl Pts',(-1.24961721838639,-0.0171963166387619,
1.1189234363026));
#23429=CARTESIAN_POINT('Ctrl Pts',(-1.23723544723125,-0.00835451937604592,
1.13139370287006));
#23430=CARTESIAN_POINT('Ctrl Pts',(-1.22409607597286,-3.12160393020622E-11,
1.14453307412866));
#23431=CARTESIAN_POINT('',(-1.08053472770428,0.042157609369957,1.28727233489076));
#23432=CARTESIAN_POINT('Ctrl Pts',(-1.08053472770428,0.0421576093699571,
1.28727233489076));
#23433=CARTESIAN_POINT('Ctrl Pts',(-1.18019989616608,0.024279158719655,
1.39987124007464));
#23434=CARTESIAN_POINT('Ctrl Pts',(-1.26544208722232,-0.0166569869072256,
1.50346488650363));
#23435=CARTESIAN_POINT('Ctrl Pts',(-1.42418037408903,-0.16009648734447,
1.715480776583));
#23436=CARTESIAN_POINT('Ctrl Pts',(-1.48987049850469,-0.275079075974332,
1.81902921434248));
#23437=CARTESIAN_POINT('Ctrl Pts',(-1.53333167412,-0.425598593400271,1.90869858745619));
#23438=CARTESIAN_POINT('Ctrl Pts',(-1.22409607597286,-3.12160393020622E-11,
1.14453307412866));
#23439=CARTESIAN_POINT('Ctrl Pts',(-1.21384438765874,0.00651841905088611,
1.15478476244295));
#23440=CARTESIAN_POINT('Ctrl Pts',(-1.20312882189276,0.0127305674258041,
1.16544721218023));
#23441=CARTESIAN_POINT('Ctrl Pts',(-1.17324021107686,0.0280274542414138,
1.19509600545493));
#23442=CARTESIAN_POINT('Ctrl Pts',(-1.15484454191168,0.0355561559109111,
1.21324740617458));
#23443=CARTESIAN_POINT('Ctrl Pts',(-1.12241703607502,0.0433677241466843,
1.24538218411131));
#23444=CARTESIAN_POINT('Ctrl Pts',(-1.10404988380787,0.0455044376575774,
1.26364457695047));
#23445=CARTESIAN_POINT('Ctrl Pts',(-1.08053472770428,0.0421576093699571,
1.28727233489076));
#23446=CARTESIAN_POINT('Ctrl Pts',(-1.08053472770428,0.0421576093699571,
1.28727233489076));
#23447=CARTESIAN_POINT('Ctrl Pts',(-1.30462473967982,0.00195919018135112,
1.54044292999951));
#23448=CARTESIAN_POINT('Ctrl Pts',(-1.45580038421926,-0.154805815536382,
1.74808806061869));
#23449=CARTESIAN_POINT('Ctrl Pts',(-1.5340616613226,-0.428137407783241,
1.91020772674828));
#23450=CARTESIAN_POINT('Ctrl Pts',(-1.07622999908393,0.0853753293366668,
1.28727233489076));
#23451=CARTESIAN_POINT('Ctrl Pts',(-1.30138937207125,0.0542581740029554,
1.54044292999951));
#23452=CARTESIAN_POINT('Ctrl Pts',(-1.45848408198029,-0.0960667204863548,
1.74808806061869));
#23453=CARTESIAN_POINT('Ctrl Pts',(-1.54751412881105,-0.365599354131263,
1.91020772674828));
#23454=CARTESIAN_POINT('Ctrl Pts',(-1.07192527046357,0.128593049303376,
1.28727233489076));
#23455=CARTESIAN_POINT('Ctrl Pts',(-1.29815400446268,0.10655715782456,1.54044292999952));
#23456=CARTESIAN_POINT('Ctrl Pts',(-1.46116777974132,-0.0373276254363268,
1.74808806061869));
#23457=CARTESIAN_POINT('Ctrl Pts',(-1.56096659629949,-0.303061300479284,
1.91020772674828));
#23458=CARTESIAN_POINT('Ctrl Pts',(-1.06762054184321,0.171810769270086,
1.28727233489076));
#23459=CARTESIAN_POINT('Ctrl Pts',(-1.29491863685411,0.158856141646164,
1.54044292999951));
#23460=CARTESIAN_POINT('Ctrl Pts',(-1.46385147750235,0.0214114696136999,
1.74808806061869));
#23461=CARTESIAN_POINT('Ctrl Pts',(-1.57441906378793,-0.240523246827305,
1.91020772674828));
#23462=CARTESIAN_POINT('Ctrl Pts',(-1.08053472770428,0.0421576093699571,
1.28727233489076));
#23463=CARTESIAN_POINT('Ctrl Pts',(-1.07899219081063,0.0637496973860188,
1.28797191329046));
#23464=CARTESIAN_POINT('Ctrl Pts',(-1.07715333835806,0.0853207093795665,
1.28831907556383));
#23465=CARTESIAN_POINT('Ctrl Pts',(-1.07501072349525,0.106872735707655,
1.288319084765));
#23466=CARTESIAN_POINT('Ctrl Pts',(-1.07285470149866,0.128559621036833,
1.28831909402374));
#23467=CARTESIAN_POINT('Ctrl Pts',(-1.07039324377381,0.150205375722343,
1.28796761487395));
#23468=CARTESIAN_POINT('Ctrl Pts',(-1.06762054184321,0.171810769270086,
1.28727233489076));
#23469=CARTESIAN_POINT('Origin',(0.,0.,1.37171309575435));
#23470=CARTESIAN_POINT('',(-1.20742290720348,0.36490527784414,1.10727038327973));
#23471=CARTESIAN_POINT('Ctrl Pts',(-1.86363850813291,-0.0276890267571663,
1.63615580822897));
#23472=CARTESIAN_POINT('Ctrl Pts',(-1.80655480211394,0.069823936699024,
1.5847793405578));
#23473=CARTESIAN_POINT('Ctrl Pts',(-1.74187241700952,0.148691945288576,
1.5334368554465));
#23474=CARTESIAN_POINT('Ctrl Pts',(-1.59669345888591,0.274785130849269,
1.4207678259124));
#23475=CARTESIAN_POINT('Ctrl Pts',(-1.51444831269986,0.320436333138579,
1.35830292226018));
#23476=CARTESIAN_POINT('Ctrl Pts',(-1.35321270714142,0.366271065016131,
1.23020598103184));
#23477=CARTESIAN_POINT('Ctrl Pts',(-1.2795761902763,0.371649422530894,1.1696137009149));
#23478=CARTESIAN_POINT('Ctrl Pts',(-1.20742290720348,0.364905277844141,
1.10727038327973));
#23479=CARTESIAN_POINT('Origin',(0.,0.,1.10727038327973));
#23480=CARTESIAN_POINT('Ctrl Pts',(-0.958722904333223,0.492368803403902,
1.28318567027397));
#23481=CARTESIAN_POINT('Ctrl Pts',(-1.17966054547972,0.551909716442827,
1.53751096017971));
#23482=CARTESIAN_POINT('Ctrl Pts',(-1.38346957888851,0.474301142999538,
1.74607168007007));
#23483=CARTESIAN_POINT('Ctrl Pts',(-1.57015000455958,0.259543083074033,
1.90886782994505));
#23484=CARTESIAN_POINT('Ctrl Pts',(-0.972472836356931,0.497730308181424,
1.26847940010162));
#23485=CARTESIAN_POINT('Ctrl Pts',(-1.196516618136,0.557797896845799,1.51987665322458));
#23486=CARTESIAN_POINT('Ctrl Pts',(-1.40288697684033,0.478816264707968,
1.72611612827484));
#23487=CARTESIAN_POINT('Ctrl Pts',(-1.59185117960571,0.260856494176603,
1.88704325648016));
#23488=CARTESIAN_POINT('Ctrl Pts',(-0.996638068239392,0.510779460904229,
1.24117819097188));
#23489=CARTESIAN_POINT('Ctrl Pts',(-1.22627731830139,0.572460097309862,
1.48716579746039));
#23490=CARTESIAN_POINT('Ctrl Pts',(-1.43799804358595,0.491635127338186,
1.68888670640878));
#23491=CARTESIAN_POINT('Ctrl Pts',(-1.63180052564183,0.268313724592159,
1.84634350908918));
#23492=CARTESIAN_POINT('Ctrl Pts',(-1.04217697649275,0.557803663431838,
1.18072535874296));
#23493=CARTESIAN_POINT('Ctrl Pts',(-1.28344787385866,0.62733559714006,1.41461088358276));
#23494=CARTESIAN_POINT('Ctrl Pts',(-1.50844372983685,0.546077997260112,
1.60644436926605));
#23495=CARTESIAN_POINT('Ctrl Pts',(-1.71730828939987,0.314053900652125,
1.75613814413928));
#23496=CARTESIAN_POINT('Ctrl Pts',(-1.07063174084474,0.608738508149426,
1.13430117558029));
#23497=CARTESIAN_POINT('Ctrl Pts',(-1.32002833380447,0.687608854742561,
1.35902160674437));
#23498=CARTESIAN_POINT('Ctrl Pts',(-1.55649910176849,0.608917570976486,
1.54332567193681));
#23499=CARTESIAN_POINT('Ctrl Pts',(-1.78021953810235,0.372863601758235,
1.68715809360677));
#23500=CARTESIAN_POINT('Ctrl Pts',(-1.08812946536139,0.649605006049397,
1.10192284729582));
#23501=CARTESIAN_POINT('Ctrl Pts',(-1.34295142581462,0.736085457637467,
1.32027771712106));
#23502=CARTESIAN_POINT('Ctrl Pts',(-1.58796351671871,0.660325994321482,
1.49933702411959));
#23503=CARTESIAN_POINT('Ctrl Pts',(-1.82316573807367,0.42232661610144,1.63910076829143));
#23504=CARTESIAN_POINT('',(-0.962275025729455,0.493314642657339,1.28727233489076));
#23505=CARTESIAN_POINT('',(-1.08521613661244,0.642908916934723,1.10727038327973));
#23506=CARTESIAN_POINT('Ctrl Pts',(-0.962275025729456,0.493314642657339,
1.28727233489076));
#23507=CARTESIAN_POINT('Ctrl Pts',(-0.992714976574408,0.505155444616818,
1.25478273943461));
#23508=CARTESIAN_POINT('Ctrl Pts',(-1.0134702004971,0.522900410114029,1.22829923781261));
#23509=CARTESIAN_POINT('Ctrl Pts',(-1.0509553613873,0.572202237707381,1.17205963503414));
#23510=CARTESIAN_POINT('Ctrl Pts',(-1.0691927306701,0.603178396560383,1.14130666672619));
#23511=CARTESIAN_POINT('Ctrl Pts',(-1.08521613661244,0.642908916934723,
1.10727038327973));
#23512=CARTESIAN_POINT('Ctrl Pts',(-0.962275025729455,0.493314642657339,
1.28727233489076));
#23513=CARTESIAN_POINT('Ctrl Pts',(-1.06019965524839,0.519074140629024,
1.39987124007464));
#23514=CARTESIAN_POINT('Ctrl Pts',(-1.15475382712427,0.517846241724568,
1.50346488650363));
#23515=CARTESIAN_POINT('Ctrl Pts',(-1.35913828497575,0.454602843714802,
1.715480776583));
#23516=CARTESIAN_POINT('Ctrl Pts',(-1.46714441944577,0.377981286365637,
1.81902921434248));
#23517=CARTESIAN_POINT('Ctrl Pts',(-1.5699559447672,0.259766273896474,1.90869858745619));
#23518=CARTESIAN_POINT('Ctrl Pts',(-1.08521613661244,0.642908916934723,
1.10727038327973));
#23519=CARTESIAN_POINT('Ctrl Pts',(-1.16760035714812,0.668710261798002,
1.18103565901041));
#23520=CARTESIAN_POINT('Ctrl Pts',(-1.25518160519554,0.6813555858353,1.25302429310884));
#23521=CARTESIAN_POINT('Ctrl Pts',(-1.44098614169379,0.665371573464,1.3926078838987));
#23522=CARTESIAN_POINT('Ctrl Pts',(-1.53389259595494,0.635301149560143,
1.45574709063854));
#23523=CARTESIAN_POINT('Ctrl Pts',(-1.69239761845936,0.541698310562581,
1.55895701082585));
#23524=CARTESIAN_POINT('Ctrl Pts',(-1.75616935678545,0.489122861296321,
1.59904902099409));
#23525=CARTESIAN_POINT('Ctrl Pts',(-1.81394816223928,0.428377445609995,
1.63615580822897));
#23526=CARTESIAN_POINT('Ctrl Pts',(-1.21487793679797,0.362330138275323,
1.10149705943221));
#23527=CARTESIAN_POINT('Ctrl Pts',(-1.48329895916361,0.383459937582892,
1.31979778023781));
#23528=CARTESIAN_POINT('Ctrl Pts',(-1.70227260218965,0.249644960941919,
1.49880741124996));
#23529=CARTESIAN_POINT('Ctrl Pts',(-1.8717988658761,-0.0391147916475981,
1.63852595246866));
#23530=CARTESIAN_POINT('Ctrl Pts',(-1.18333690797345,0.373447482460584,
1.12583385309083));
#23531=CARTESIAN_POINT('Ctrl Pts',(-1.44573672483851,0.398305182537798,
1.34892944774501));
#23532=CARTESIAN_POINT('Ctrl Pts',(-1.66212671668266,0.270675994878907,
1.53186602370529));
#23533=CARTESIAN_POINT('Ctrl Pts',(-1.83255854794258,-0.00930365130124231,
1.6746483889292));
#23534=CARTESIAN_POINT('Ctrl Pts',(-1.13169790455625,0.386758017000774,
1.16764044916317));
#23535=CARTESIAN_POINT('Ctrl Pts',(-1.38402127269754,0.416680587119741,
1.39897336709084));
#23536=CARTESIAN_POINT('Ctrl Pts',(-1.59542335194443,0.29867037569466,1.58871211231351));
#23537=CARTESIAN_POINT('Ctrl Pts',(-1.76604232095016,0.0327265383253359,
1.7367627568762));
#23538=CARTESIAN_POINT('Ctrl Pts',(-1.06341115236231,0.391671741837562,
1.22801607619329));
#23539=CARTESIAN_POINT('Ctrl Pts',(-1.30168216224368,0.425665904909548,
1.47139032317726));
#23540=CARTESIAN_POINT('Ctrl Pts',(-1.50457544636212,0.318647566754323,
1.67096220367118));
#23541=CARTESIAN_POINT('Ctrl Pts',(-1.67209124376878,0.0706042875438534,
1.82672793765152));
#23542=CARTESIAN_POINT('Ctrl Pts',(-1.0286884268729,0.38218165487343,1.263527751515));
#23543=CARTESIAN_POINT('Ctrl Pts',(-1.25929056133868,0.415770412604395,
1.51397381108001));
#23544=CARTESIAN_POINT('Ctrl Pts',(-1.45588630034145,0.312692596804324,
1.71945276482243));
#23545=CARTESIAN_POINT('Ctrl Pts',(-1.61878272768801,0.0729619965738858,
1.8797604367197));
#23546=CARTESIAN_POINT('Ctrl Pts',(-1.01098164381094,0.373486051297297,
1.28318517919159));
#23547=CARTESIAN_POINT('Ctrl Pts',(-1.23750736860246,0.40602648967972,1.53754499301511));
#23548=CARTESIAN_POINT('Ctrl Pts',(-1.43052436008972,0.304436793685257,
1.74612783237315));
#23549=CARTESIAN_POINT('Ctrl Pts',(-1.59003261827273,0.0687169633139079,
1.90893369726572));
#23550=CARTESIAN_POINT('',(-1.01462217612883,0.373997862975654,1.28727233489076));
#23551=CARTESIAN_POINT('Ctrl Pts',(-1.20742290720348,0.364905277844141,
1.10727038327973));
#23552=CARTESIAN_POINT('Ctrl Pts',(-1.18311862080923,0.3736159450907,1.12801545944054));
#23553=CARTESIAN_POINT('Ctrl Pts',(-1.15609247800018,0.381365818655266,
1.15133239961433));
#23554=CARTESIAN_POINT('Ctrl Pts',(-1.10715678825378,0.389206856698375,
1.19509600545556));
#23555=CARTESIAN_POINT('Ctrl Pts',(-1.08733497046134,0.390682503085297,
1.2132474061751));
#23556=CARTESIAN_POINT('Ctrl Pts',(-1.05408067239149,0.388091095569761,
1.24538218411098));
#23557=CARTESIAN_POINT('Ctrl Pts',(-1.03595219175499,0.38444746868904,1.26364457695016));
#23558=CARTESIAN_POINT('Ctrl Pts',(-1.01462217612883,0.373997862975654,
1.28727233489076));
#23559=CARTESIAN_POINT('Ctrl Pts',(-1.01462217612883,0.373997862975654,
1.28727233489076));
#23560=CARTESIAN_POINT('Ctrl Pts',(-1.11493412912611,0.387792676785359,
1.39987124007464));
#23561=CARTESIAN_POINT('Ctrl Pts',(-1.20865423507634,0.375201374409042,
1.50346488650363));
#23562=CARTESIAN_POINT('Ctrl Pts',(-1.40394856048621,0.287835131123856,
1.715480776583));
#23563=CARTESIAN_POINT('Ctrl Pts',(-1.50195515531182,0.198779555753984,
1.81902921434248));
#23564=CARTESIAN_POINT('Ctrl Pts',(-1.58980227845634,0.0690572297370887,
1.90869858745619));
#23565=CARTESIAN_POINT('Ctrl Pts',(-1.01462217612883,0.373997862975653,
1.28727233489076));
#23566=CARTESIAN_POINT('Ctrl Pts',(-1.24016643693111,0.405014516431691,
1.54044292999952));
#23567=CARTESIAN_POINT('Ctrl Pts',(-1.43238606966553,0.302637979515068,
1.74808806061869));
#23568=CARTESIAN_POINT('Ctrl Pts',(-1.59128107433209,0.0668682522257823,
1.91020772674828));
#23569=CARTESIAN_POINT('Ctrl Pts',(-0.997173125995706,0.413770122869549,
1.28727233489076));
#23570=CARTESIAN_POINT('Ctrl Pts',(-1.22092814469495,0.453754022216744,
1.54044292999952));
#23571=CARTESIAN_POINT('Ctrl Pts',(-1.41678703930426,0.3593314868396,1.74808806061869));
#23572=CARTESIAN_POINT('Ctrl Pts',(-1.58474980982363,0.130502516738118,
1.91020772674828));
#23573=CARTESIAN_POINT('Ctrl Pts',(-0.979724075862581,0.453542382763444,
1.28727233489076));
#23574=CARTESIAN_POINT('Ctrl Pts',(-1.2016898524588,0.502493528001797,1.54044292999952));
#23575=CARTESIAN_POINT('Ctrl Pts',(-1.40118800894299,0.416024994164134,
1.74808806061869));
#23576=CARTESIAN_POINT('Ctrl Pts',(-1.57821854531517,0.194136781250453,
1.91020772674828));
#23577=CARTESIAN_POINT('Ctrl Pts',(-0.962275025729455,0.493314642657339,
1.28727233489076));
#23578=CARTESIAN_POINT('Ctrl Pts',(-1.18245156022264,0.55123303378685,1.54044292999952));
#23579=CARTESIAN_POINT('Ctrl Pts',(-1.38558897858172,0.472718501488667,
1.74808806061869));
#23580=CARTESIAN_POINT('Ctrl Pts',(-1.5716872808067,0.257771045762789,1.91020772674828));
#23581=CARTESIAN_POINT('Ctrl Pts',(-1.01462217612883,0.373997862975654,
1.28727233489076));
#23582=CARTESIAN_POINT('Ctrl Pts',(-1.00648281422349,0.394056488869176,
1.28797191329047));
#23583=CARTESIAN_POINT('Ctrl Pts',(-0.998068152324093,0.414003503730718,
1.28831907556383));
#23584=CARTESIAN_POINT('Ctrl Pts',(-0.989370462098314,0.433838594404394,
1.288319084765));
#23585=CARTESIAN_POINT('Ctrl Pts',(-0.980618347207407,0.453797800577666,
1.28831909402374));
#23586=CARTESIAN_POINT('Ctrl Pts',(-0.971588455744705,0.473623504353535,
1.28796761487395));
#23587=CARTESIAN_POINT('Ctrl Pts',(-0.962275025729455,0.493314642657339,
1.28727233489076));
#23588=CARTESIAN_POINT('Origin',(0.,0.,1.37171309575435));
#23589=CARTESIAN_POINT('',(-1.03556549162895,0.720159740047643,1.10727038327973));
#23590=CARTESIAN_POINT('Ctrl Pts',(-1.78098192700405,0.549562141057369,
1.63615580822897));
#23591=CARTESIAN_POINT('Ctrl Pts',(-1.70079633666886,0.620893161259203,
1.58735805514606));
#23592=CARTESIAN_POINT('Ctrl Pts',(-1.61925404078159,0.67413336725827,1.53858095020834));
#23593=CARTESIAN_POINT('Ctrl Pts',(-1.44461319502359,0.751969574388254,
1.42806953503213));
#23594=CARTESIAN_POINT('Ctrl Pts',(-1.35007152673689,0.772017157909612,
1.36461306044571));
#23595=CARTESIAN_POINT('Ctrl Pts',(-1.1777963531315,0.7674790066995,1.23357020765531));
#23596=CARTESIAN_POINT('Ctrl Pts',(-1.10397180136272,0.749676646324454,
1.17136442658356));
#23597=CARTESIAN_POINT('Ctrl Pts',(-1.03556549162895,0.720159740047643,
1.10727038327973));
#23598=CARTESIAN_POINT('Origin',(0.,0.,1.10727038327973));
#23599=CARTESIAN_POINT('Ctrl Pts',(-0.759649337735664,0.764532229233201,
1.28318567027397));
#23600=CARTESIAN_POINT('Ctrl Pts',(-0.951374367053292,0.889432488376416,
1.53751096017971));
#23601=CARTESIAN_POINT('Ctrl Pts',(-1.16919064445971,0.87860280381325,1.74607168007007));
#23602=CARTESIAN_POINT('Ctrl Pts',(-1.41309816995491,0.732043175543704,
1.90886782994505));
#23603=CARTESIAN_POINT('Ctrl Pts',(-0.771069504093749,0.773880285955837,
1.26847940010162));
#23604=CARTESIAN_POINT('Ctrl Pts',(-0.965585896981724,0.900241293626992,
1.51987665322458));
#23605=CARTESIAN_POINT('Ctrl Pts',(-1.18626243797171,0.888897245689575,
1.72611612827484));
#23606=CARTESIAN_POINT('Ctrl Pts',(-1.43333134754249,0.739998335618538,
1.88704325648016));
#23607=CARTESIAN_POINT('Ctrl Pts',(-0.790019380359266,0.793756470105417,
1.24117952306876));
#23608=CARTESIAN_POINT('Ctrl Pts',(-0.989358920654663,0.923380672132903,
1.48716712955727));
#23609=CARTESIAN_POINT('Ctrl Pts',(-1.2156928538318,0.911936310735737,1.68888851879236));
#23610=CARTESIAN_POINT('Ctrl Pts',(-1.46902007592139,0.759433295933264,
1.84634532147277));
#23611=CARTESIAN_POINT('Ctrl Pts',(-0.818798433422957,0.852549487780084,
1.18072779772815));
#23612=CARTESIAN_POINT('Ctrl Pts',(-1.02677414338759,0.993235093958051,
1.41461332256795));
#23613=CARTESIAN_POINT('Ctrl Pts',(-1.26586652272339,0.985480669746802,
1.60644767971083));
#23614=CARTESIAN_POINT('Ctrl Pts',(-1.53620791207528,0.829355339157892,
1.75614145458406));
#23615=CARTESIAN_POINT('Ctrl Pts',(-0.830120749534189,0.909788127533561,
1.13430117558029));
#23616=CARTESIAN_POINT('Ctrl Pts',(-1.04293872696083,1.06186607016719,1.35902160674437));
#23617=CARTESIAN_POINT('Ctrl Pts',(-1.29215273573923,1.06009969793961,1.54332567193681));
#23618=CARTESIAN_POINT('Ctrl Pts',(-1.57786820262105,0.9047324491334,1.68715809360677));
#23619=CARTESIAN_POINT('Ctrl Pts',(-0.834133632104406,0.954061570898026,
1.10192284729582));
#23620=CARTESIAN_POINT('Ctrl Pts',(-1.04975978886662,1.115053684233,1.32027771712106));
#23621=CARTESIAN_POINT('Ctrl Pts',(-1.30619109614143,1.11871505289201,1.49933702411959));
#23622=CARTESIAN_POINT('Ctrl Pts',(-1.60342755392882,0.965045676875065,
1.63910076829143));
#23623=CARTESIAN_POINT('',(-0.762735325532963,0.766529441696069,1.28727233489076));
#23624=CARTESIAN_POINT('',(-0.833432097145889,0.946792943618196,1.10727038327973));
#23625=CARTESIAN_POINT('Ctrl Pts',(-0.762735325532963,0.766529441696069,
1.28727233489076));
#23626=CARTESIAN_POINT('Ctrl Pts',(-0.788026430107593,0.787197175677101,
1.25478273943417));
#23627=CARTESIAN_POINT('Ctrl Pts',(-0.80228232516309,0.810487357658964,
1.22829923781215));
#23628=CARTESIAN_POINT('Ctrl Pts',(-0.822697729112326,0.868959733810234,
1.17205963503243));
#23629=CARTESIAN_POINT('Ctrl Pts',(-0.830470338502341,0.90405546857811,
1.14130666672486));
#23630=CARTESIAN_POINT('Ctrl Pts',(-0.833432097145889,0.946792943618196,
1.10727038327973));
#23631=CARTESIAN_POINT('Ctrl Pts',(-0.762735325532963,0.766529441696069,
1.28727233489076));
#23632=CARTESIAN_POINT('Ctrl Pts',(-0.847907059902912,0.821288554787752,
1.39987124007464));
#23633=CARTESIAN_POINT('Ctrl Pts',(-0.938212862837218,0.849339599532016,
1.50346488650363));
#23634=CARTESIAN_POINT('Ctrl Pts',(-1.15213731807335,0.852349824604396,
1.715480776583));
#23635=CARTESIAN_POINT('Ctrl Pts',(-1.27853461941729,0.812854124246773,
1.81902921434248));
#23636=CARTESIAN_POINT('Ctrl Pts',(-1.41284463836769,0.732195474855993,
1.90869858745619));
#23637=CARTESIAN_POINT('Ctrl Pts',(-0.833432097145889,0.946792943618196,
1.10727038327973));
#23638=CARTESIAN_POINT('Ctrl Pts',(-0.903811092885819,0.996789604993491,
1.18103565901046));
#23639=CARTESIAN_POINT('Ctrl Pts',(-0.983198189519745,1.03588011685507,
1.25302429310894));
#23640=CARTESIAN_POINT('Ctrl Pts',(-1.16484813617473,1.07809517714268,1.39260788389885));
#23641=CARTESIAN_POINT('Ctrl Pts',(-1.26249969692003,1.07820617779494,1.45574709063867));
#23642=CARTESIAN_POINT('Ctrl Pts',(-1.44217179941028,1.03816533347019,1.55895701082593));
#23643=CARTESIAN_POINT('Ctrl Pts',(-1.51906903401087,1.00786966075199,1.59904902099412));
#23644=CARTESIAN_POINT('Ctrl Pts',(-1.59279130921887,0.967951970128402,
1.63615580822897));
#23645=CARTESIAN_POINT('Ctrl Pts',(-1.04334803864884,0.720016914634041,
1.1015723109602));
#23646=CARTESIAN_POINT('Ctrl Pts',(-1.29208090893698,0.823064346331375,
1.31988785480615));
#23647=CARTESIAN_POINT('Ctrl Pts',(-1.54167481933166,0.763481187915701,
1.4989096332868));
#23648=CARTESIAN_POINT('Ctrl Pts',(-1.79212976983288,0.541267439387018,
1.63863764640214));
#23649=CARTESIAN_POINT('Ctrl Pts',(-1.00993315330316,0.720837529677195,
1.12589971949673));
#23650=CARTESIAN_POINT('Ctrl Pts',(-1.25179094217685,0.825567715093928,
1.34900830339197));
#23651=CARTESIAN_POINT('Ctrl Pts',(-1.49701757504304,0.771065844731935,
1.53195557707745));
#23652=CARTESIAN_POINT('Ctrl Pts',(-1.74562013410099,0.557477346013106,
1.67474624941239));
#23653=CARTESIAN_POINT('Ctrl Pts',(-0.956735633325592,0.717530565095652,
1.16769179538367));
#23654=CARTESIAN_POINT('Ctrl Pts',(-1.1874504232267,0.823961384252212,1.39903449435105));
#23655=CARTESIAN_POINT('Ctrl Pts',(-1.42496257773994,0.777060632929274,
1.58878199846585));
#23656=CARTESIAN_POINT('Ctrl Pts',(-1.66940588754285,0.576871348730687,
1.73683890344256));
#23657=CARTESIAN_POINT('Ctrl Pts',(-0.890308540641222,0.701101131459803,
1.22804130170825));
#23658=CARTESIAN_POINT('Ctrl Pts',(-1.10640797973513,0.80706000931713,1.47142017171287));
#23659=CARTESIAN_POINT('Ctrl Pts',(-1.33243573819092,0.767978311363814,
1.67099665961543));
#23660=CARTESIAN_POINT('Ctrl Pts',(-1.56839818009432,0.583845206097258,
1.82676536339563));
#23661=CARTESIAN_POINT('Ctrl Pts',(-0.860233953705641,0.681352489183287,
1.2635364344865));
#23662=CARTESIAN_POINT('Ctrl Pts',(-1.06916866744104,0.784556163294569,
1.51398418220584));
#23663=CARTESIAN_POINT('Ctrl Pts',(-1.28799335847826,0.747275208483434,
1.71946457116169));
#23664=CARTESIAN_POINT('Ctrl Pts',(-1.51699586639177,0.569616647707412,
1.87977332297458));
#23665=CARTESIAN_POINT('Ctrl Pts',(-0.846087143187382,0.667616851769879,
1.28318517919043));
#23666=CARTESIAN_POINT('Ctrl Pts',(-1.05147036139455,0.768564946360843,
1.53754499301448));
#23667=CARTESIAN_POINT('Ctrl Pts',(-1.26643337142019,0.731592934569703,
1.74612783237292));
#23668=CARTESIAN_POINT('Ctrl Pts',(-1.4909761732643,0.556700816396459,1.90893369726574));
#23669=CARTESIAN_POINT('',(-0.849391336665505,0.669228599956957,1.28727233489076));
#23670=CARTESIAN_POINT('Ctrl Pts',(-1.03556549162895,0.720159740047643,
1.10727038327973));
#23671=CARTESIAN_POINT('Ctrl Pts',(-1.00975899746819,0.720933639361786,
1.12801545944061));
#23672=CARTESIAN_POINT('Ctrl Pts',(-0.981660765603669,0.719952669695422,
1.15133239961436));
#23673=CARTESIAN_POINT('Ctrl Pts',(-0.932697144982725,0.712287980257843,
1.19509600545502));
#23674=CARTESIAN_POINT('Ctrl Pts',(-0.91338947619488,0.707566124812641,
1.21324740617476));
#23675=CARTESIAN_POINT('Ctrl Pts',(-0.882563548281158,0.694825406568518,
1.24538218411192));
#23676=CARTESIAN_POINT('Ctrl Pts',(-0.866448281268894,0.685758102881577,
1.26364457695098));
#23677=CARTESIAN_POINT('Ctrl Pts',(-0.849391336665505,0.669228599956957,
1.28727233489076));
#23678=CARTESIAN_POINT('Ctrl Pts',(-0.849391336665505,0.669228599956957,
1.28727233489076));
#23679=CARTESIAN_POINT('Ctrl Pts',(-0.940530841324424,0.713346345736856,
1.39987124007464));
#23680=CARTESIAN_POINT('Ctrl Pts',(-1.03355488521186,0.73033241101646,1.50346488650363));
#23681=CARTESIAN_POINT('Ctrl Pts',(-1.2462884798982,0.707591441492497,1.715480776583));
#23682=CARTESIAN_POINT('Ctrl Pts',(-1.36701797678012,0.653180259586498,
1.81902921434248));
#23683=CARTESIAN_POINT('Ctrl Pts',(-1.49065195897357,0.55695325007777,1.90869858745619));
#23684=CARTESIAN_POINT('Ctrl Pts',(-0.849391336665504,0.669228599956957,
1.28727233489076));
#23685=CARTESIAN_POINT('Ctrl Pts',(-1.05431200258793,0.768424199911631,
1.54044292999952));
#23686=CARTESIAN_POINT('Ctrl Pts',(-1.26875982659235,0.73045746052879,1.74808806061869));
#23687=CARTESIAN_POINT('Ctrl Pts',(-1.49273480867877,0.555328381808437,
1.91020772674828));
#23688=CARTESIAN_POINT('Ctrl Pts',(-0.820505999621324,0.701662213869995,
1.28727233489076));
#23689=CARTESIAN_POINT('Ctrl Pts',(-1.02095396380933,0.808833265245786,
1.54044292999952));
#23690=CARTESIAN_POINT('Ctrl Pts',(-1.23640500988538,0.779555824624011,
1.74808806061869));
#23691=CARTESIAN_POINT('Ctrl Pts',(-1.46685913784949,0.613829892004671,
1.91020772674828));
#23692=CARTESIAN_POINT('Ctrl Pts',(-0.791620662577143,0.734095827783032,
1.28727233489076));
#23693=CARTESIAN_POINT('Ctrl Pts',(-0.98759592503072,0.849242330579942,
1.54044292999952));
#23694=CARTESIAN_POINT('Ctrl Pts',(-1.20405019317841,0.828654188719233,
1.74808806061869));
#23695=CARTESIAN_POINT('Ctrl Pts',(-1.4409834670202,0.672331402200905,1.91020772674828));
#23696=CARTESIAN_POINT('Ctrl Pts',(-0.762735325532963,0.766529441696069,
1.28727233489076));
#23697=CARTESIAN_POINT('Ctrl Pts',(-0.954237886252114,0.889651395914097,
1.54044292999952));
#23698=CARTESIAN_POINT('Ctrl Pts',(-1.17169537647143,0.877752552814453,
1.74808806061869));
#23699=CARTESIAN_POINT('Ctrl Pts',(-1.41510779619092,0.730832912397138,
1.91020772674828));
#23700=CARTESIAN_POINT('Ctrl Pts',(-0.849391336665504,0.669228599956957,
1.28727233489076));
#23701=CARTESIAN_POINT('Ctrl Pts',(-0.835451887202037,0.685790285668798,
1.28797191329046));
#23702=CARTESIAN_POINT('Ctrl Pts',(-0.82128510159093,0.702160750604672,
1.28831907556383));
#23703=CARTESIAN_POINT('Ctrl Pts',(-0.806883726521851,0.718337308749603,
1.288319084765));
#23704=CARTESIAN_POINT('Ctrl Pts',(-0.792392236721721,0.734615089602754,
1.28831909402374));
#23705=CARTESIAN_POINT('Ctrl Pts',(-0.777677820212499,0.750680064449589,
1.28796761487395));
#23706=CARTESIAN_POINT('Ctrl Pts',(-0.762735325532963,0.766529441696069,
1.28727233489076));
#23707=CARTESIAN_POINT('Origin',(0.,0.,1.37171309575435));
#23708=CARTESIAN_POINT('',(-0.762339710524744,1.00491994924733,1.10727038327973));
#23709=CARTESIAN_POINT('Ctrl Pts',(-1.52399042602929,1.07301833748062,1.63615580822897));
#23710=CARTESIAN_POINT('Ctrl Pts',(-1.42568690035968,1.11607945893995,1.58735805514612));
#23711=CARTESIAN_POINT('Ctrl Pts',(-1.33168344006467,1.14151594859478,1.5385809502084));
#23712=CARTESIAN_POINT('Ctrl Pts',(-1.14153741491427,1.16157559133822,1.42806953503213));
#23713=CARTESIAN_POINT('Ctrl Pts',(-1.04542790122454,1.15142699410503,1.36461306044571));
#23714=CARTESIAN_POINT('Ctrl Pts',(-0.882986840618225,1.09387499947176,
1.23357020765531));
#23715=CARTESIAN_POINT('Ctrl Pts',(-0.818276751491845,1.05413090753297,
1.17136442658356));
#23716=CARTESIAN_POINT('Ctrl Pts',(-0.762339710524744,1.00491994924733,
1.10727038327973));
#23717=CARTESIAN_POINT('Origin',(0.,0.,1.10727038327973));
#23718=CARTESIAN_POINT('Ctrl Pts',(-0.486216001172379,0.96185791365589,
1.28318567027397));
#23719=CARTESIAN_POINT('Ctrl Pts',(-0.629961036964704,1.13989141130718,
1.53751096017972));
#23720=CARTESIAN_POINT('Ctrl Pts',(-0.84046318352097,1.19690070060403,1.74607168007008));
#23721=CARTESIAN_POINT('Ctrl Pts',(-1.11772244084118,1.13288578154644,1.90886782994506));
#23722=CARTESIAN_POINT('Ctrl Pts',(-0.496846021492854,0.978417321314553,
1.26357731004417));
#23723=CARTESIAN_POINT('Ctrl Pts',(-0.643585521081937,1.15940183561927,
1.51399891879436));
#23724=CARTESIAN_POINT('Ctrl Pts',(-0.857895946504486,1.21707904013549,
1.71946418982835));
#23725=CARTESIAN_POINT('Ctrl Pts',(-1.14010192848643,1.15131005161592,1.87976839865855));
#23726=CARTESIAN_POINT('Ctrl Pts',(-0.510215828707944,1.01174306480633,
1.22814964935774));
#23727=CARTESIAN_POINT('Ctrl Pts',(-0.661178469414083,1.19911435608045,
1.47151698835253));
#23728=CARTESIAN_POINT('Ctrl Pts',(-0.882459067352746,1.25929534063486,
1.67109028087187));
#23729=CARTESIAN_POINT('Ctrl Pts',(-1.17406335818981,1.19229498704013,1.82686350557264));
#23730=CARTESIAN_POINT('Ctrl Pts',(-0.513157287930765,1.07994419721084,
1.16792318405107));
#23731=CARTESIAN_POINT('Ctrl Pts',(-0.667766287860981,1.2814248116504,1.39927998114664));
#23732=CARTESIAN_POINT('Ctrl Pts',(-0.899659869879336,1.35048605385199,
1.58904519906558));
#23733=CARTESIAN_POINT('Ctrl Pts',(-1.20898915642793,1.28706885932715,1.73712239616959));
#23734=CARTESIAN_POINT('Ctrl Pts',(-0.505885563397483,1.13261799505841,
1.12620659350917));
#23735=CARTESIAN_POINT('Ctrl Pts',(-0.661308446532945,1.34530596753016,
1.34934531900259));
#23736=CARTESIAN_POINT('Ctrl Pts',(-0.90016534752349,1.42259827975627,1.53232296148775));
#23737=CARTESIAN_POINT('Ctrl Pts',(-1.22248177762695,1.3643546712912,1.67514376227795));
#23738=CARTESIAN_POINT('Ctrl Pts',(-0.498486987186291,1.16512794184932,
1.10192284729582));
#23739=CARTESIAN_POINT('Ctrl Pts',(-0.653810349677836,1.38487268717996,
1.32027771712106));
#23740=CARTESIAN_POINT('Ctrl Pts',(-0.896559590305325,1.46759648753937,
1.4993370241196));
#23741=CARTESIAN_POINT('Ctrl Pts',(-1.22673470906876,1.41329934292755,1.63910076829144));
#23742=CARTESIAN_POINT('',(-0.488533777383804,0.964710998256926,1.28727233489076));
#23743=CARTESIAN_POINT('',(-0.500065917147829,1.15799828028599,1.10727038327973));
#23744=CARTESIAN_POINT('Ctrl Pts',(-0.488533777383804,0.964710998256926,
1.28727233489076));
#23745=CARTESIAN_POINT('Ctrl Pts',(-0.50620036615867,0.992182562457059,
1.25478273943377));
#23746=CARTESIAN_POINT('Ctrl Pts',(-0.512561466012053,1.01873815563885,
1.2282992378118));
#23747=CARTESIAN_POINT('Ctrl Pts',(-0.513908711038649,1.08065739676658,
1.17205963503343));
#23748=CARTESIAN_POINT('Ctrl Pts',(-0.510455723374509,1.11643729240398,
1.14130666672571));
#23749=CARTESIAN_POINT('Ctrl Pts',(-0.500065917147829,1.15799828028599,
1.10727038327973));
#23750=CARTESIAN_POINT('Ctrl Pts',(-0.488533777383804,0.964710998256926,
1.28727233489076));
#23751=CARTESIAN_POINT('Ctrl Pts',(-0.552615413818275,1.04310952295002,
1.39987124007464));
#23752=CARTESIAN_POINT('Ctrl Pts',(-0.629833086622262,1.09769367964031,
1.50346488650363));
#23753=CARTESIAN_POINT('Ctrl Pts',(-0.832357123065218,1.16666286599128,
1.715480776583));
#23754=CARTESIAN_POINT('Ctrl Pts',(-0.964772942765737,1.16815913695893,
1.81902921434248));
#23755=CARTESIAN_POINT('Ctrl Pts',(-1.11743425489732,1.13295228123076,1.90869858745619));
#23756=CARTESIAN_POINT('Ctrl Pts',(-0.500065917147829,1.15799828028599,
1.10727038327973));
#23757=CARTESIAN_POINT('Ctrl Pts',(-0.551550501629625,1.22729623661065,
1.18103565901047));
#23758=CARTESIAN_POINT('Ctrl Pts',(-0.614972484709036,1.28900548463589,
1.25302429310895));
#23759=CARTESIAN_POINT('Ctrl Pts',(-0.774686679112503,1.38528731335191,
1.39260788389886));
#23760=CARTESIAN_POINT('Ctrl Pts',(-0.867524531197774,1.41556887304308,
1.45574709063869));
#23761=CARTESIAN_POINT('Ctrl Pts',(-1.05077615643305,1.43300950021463,1.55895701082594));
#23762=CARTESIAN_POINT('Ctrl Pts',(-1.13327165021096,1.42795915557245,1.59904902099413));
#23763=CARTESIAN_POINT('Ctrl Pts',(-1.21572094522251,1.4127766116927,1.63615580822897));
#23764=CARTESIAN_POINT('Ctrl Pts',(-0.769785488061408,1.0071890534957,1.10157231096021));
#23765=CARTESIAN_POINT('Ctrl Pts',(-0.974501097544568,1.18205566887762,
1.31988785480615));
#23766=CARTESIAN_POINT('Ctrl Pts',(-1.23029122098199,1.2025174778094,1.4989096332868));
#23767=CARTESIAN_POINT('Ctrl Pts',(-1.53715585837368,1.06857448029104,1.63863764640214));
#23768=CARTESIAN_POINT('Ctrl Pts',(-0.727074783470151,0.994461965292039,
1.13400885567558));
#23769=CARTESIAN_POINT('Ctrl Pts',(-0.922448816386925,1.16858584308541,
1.35870212368825));
#23770=CARTESIAN_POINT('Ctrl Pts',(-1.17054629234371,1.19383871456862,1.54297833728481));
#23771=CARTESIAN_POINT('Ctrl Pts',(-1.47149928669632,1.06996683960028,1.68678245041581));
#23772=CARTESIAN_POINT('Ctrl Pts',(-0.673083751047335,0.971974682567364,
1.18052322600159));
#23773=CARTESIAN_POINT('Ctrl Pts',(-0.856229621362336,1.1438936589507,1.41439979544558));
#23774=CARTESIAN_POINT('Ctrl Pts',(-1.0936426848353,1.17420151395341,1.60622137130565));
#23775=CARTESIAN_POINT('Ctrl Pts',(-1.38546708108516,1.06281232835789,1.75589800730002));
#23776=CARTESIAN_POINT('Ctrl Pts',(-0.621030952892813,0.932030917609336,
1.24109849008298));
#23777=CARTESIAN_POINT('Ctrl Pts',(-0.791463701885433,1.09790581924279,
1.48710325590114));
#23778=CARTESIAN_POINT('Ctrl Pts',(-1.01576709402367,1.13059499103696,1.68883275601271));
#23779=CARTESIAN_POINT('Ctrl Pts',(-1.29394102274663,1.03008879377588,1.84628852230556));
#23780=CARTESIAN_POINT('Ctrl Pts',(-0.605279141158067,0.909472892481623,
1.26844862066248));
#23781=CARTESIAN_POINT('Ctrl Pts',(-0.771469550259548,1.07134082867159,
1.51987386218776));
#23782=CARTESIAN_POINT('Ctrl Pts',(-0.990137606500526,1.10338745862407,
1.72613059618619));
#23783=CARTESIAN_POINT('Ctrl Pts',(-1.26153883267189,1.00543407447983,1.88706341654737));
#23784=CARTESIAN_POINT('Ctrl Pts',(-0.598371737953918,0.89639666323125,
1.28318517919043));
#23785=CARTESIAN_POINT('Ctrl Pts',(-0.762508109189138,1.055870911185,1.53754499301448));
#23786=CARTESIAN_POINT('Ctrl Pts',(-0.978375060596135,1.08713566171041,
1.74612783237291));
#23787=CARTESIAN_POINT('Ctrl Pts',(-1.24597259217491,0.990190914807483,
1.90893369726573));
#23788=CARTESIAN_POINT('',(-0.601016155111926,0.89895057878464,1.28727233489076));
#23789=CARTESIAN_POINT('Ctrl Pts',(-0.762339710524744,1.00491994924733,
1.10727038327973));
#23790=CARTESIAN_POINT('Ctrl Pts',(-0.737557128050267,0.997681325972047,
1.12801545944073));
#23791=CARTESIAN_POINT('Ctrl Pts',(-0.711137257836933,0.988065537220461,
1.15133239961458));
#23792=CARTESIAN_POINT('Ctrl Pts',(-0.666938606676026,0.965645393507086,
1.19509600545601));
#23793=CARTESIAN_POINT('Ctrl Pts',(-0.650035056038688,0.955188244339594,
1.2132474061757));
#23794=CARTESIAN_POINT('Ctrl Pts',(-0.624654954884539,0.933545365639427,
1.24538218411151));
#23795=CARTESIAN_POINT('Ctrl Pts',(-0.612130376112959,0.919941956007105,
1.26364457695062));
#23796=CARTESIAN_POINT('Ctrl Pts',(-0.601016155111926,0.89895057878464,
1.28727233489076));
#23797=CARTESIAN_POINT('Ctrl Pts',(-0.601016155111926,0.89895057878464,
1.28727233489076));
#23798=CARTESIAN_POINT('Ctrl Pts',(-0.674061841710201,0.969072704191387,
1.39987124007464));
#23799=CARTESIAN_POINT('Ctrl Pts',(-0.757283981982513,1.01397342270847,
1.50346488650363));
#23800=CARTESIAN_POINT('Ctrl Pts',(-0.966632999495317,1.05808377148838,
1.715480776583));
#23801=CARTESIAN_POINT('Ctrl Pts',(-1.09826755410688,1.04364312863621,1.81902921434248));
#23802=CARTESIAN_POINT('Ctrl Pts',(-1.24558623976355,0.990330805779366,
1.90869858745619));
#23803=CARTESIAN_POINT('Ctrl Pts',(-0.601016155111926,0.89895057878464,
1.28727233489076));
#23804=CARTESIAN_POINT('Ctrl Pts',(-0.765254163607779,1.056615168778,1.54044292999952));
#23805=CARTESIAN_POINT('Ctrl Pts',(-0.980938531722802,1.08677467590956,
1.74808806061869));
#23806=CARTESIAN_POINT('Ctrl Pts',(-1.24806925945699,0.989429100179333,
1.91020772674828));
#23807=CARTESIAN_POINT('Ctrl Pts',(-0.563522029202552,0.920870718608735,
1.28727233489076));
#23808=CARTESIAN_POINT('Ctrl Pts',(-0.721041695541499,1.08473827279984,
1.54044292999952));
#23809=CARTESIAN_POINT('Ctrl Pts',(-0.934995043558668,1.12347180680942,
1.74808806061869));
#23810=CARTESIAN_POINT('Ctrl Pts',(-1.20538207325406,1.03707132063747,1.91020772674828));
#23811=CARTESIAN_POINT('Ctrl Pts',(-0.526027903293178,0.94279085843283,
1.28727233489076));
#23812=CARTESIAN_POINT('Ctrl Pts',(-0.676829227475217,1.11286137682168,
1.54044292999952));
#23813=CARTESIAN_POINT('Ctrl Pts',(-0.889051555394535,1.16016893770927,
1.74808806061869));
#23814=CARTESIAN_POINT('Ctrl Pts',(-1.16269488705113,1.0847135410956,1.91020772674828));
#23815=CARTESIAN_POINT('Ctrl Pts',(-0.488533777383804,0.964710998256926,
1.28727233489076));
#23816=CARTESIAN_POINT('Ctrl Pts',(-0.632616759408936,1.14098448084351,
1.54044292999952));
#23817=CARTESIAN_POINT('Ctrl Pts',(-0.843108067230401,1.19686606860912,
1.74808806061869));
#23818=CARTESIAN_POINT('Ctrl Pts',(-1.1200077008482,1.13235576155374,1.91020772674828));
#23819=CARTESIAN_POINT('Ctrl Pts',(-0.601016155111926,0.89895057878464,
1.28727233489076));
#23820=CARTESIAN_POINT('Ctrl Pts',(-0.582641108525671,0.910394151125278,
1.28797191329047));
#23821=CARTESIAN_POINT('Ctrl Pts',(-0.564108942884267,0.921585610967823,
1.28831907556383));
#23822=CARTESIAN_POINT('Ctrl Pts',(-0.545413589903933,0.932520162364073,
1.288319084765));
#23823=CARTESIAN_POINT('Ctrl Pts',(-0.526601253184359,0.943523135293236,
1.28831909402374));
#23824=CARTESIAN_POINT('Ctrl Pts',(-0.507642661237903,0.954254829541775,
1.28796761487395));
#23825=CARTESIAN_POINT('Ctrl Pts',(-0.488533777383804,0.964710998256926,
1.28727233489076));
#23826=CARTESIAN_POINT('Origin',(0.,0.,1.37171309575435));
#23827=CARTESIAN_POINT('',(-0.414490807021284,1.19131159212569,1.10727038327973));
#23828=CARTESIAN_POINT('Ctrl Pts',(-1.11782012388912,1.4914400228729,1.63615580822897));
#23829=CARTESIAN_POINT('Ctrl Pts',(-1.01102129689809,1.50201612299693,1.58735805514594));
#23830=CARTESIAN_POINT('Ctrl Pts',(-0.913758385849714,1.49715899547352,
1.53858095020821));
#23831=CARTESIAN_POINT('Ctrl Pts',(-0.726719999074283,1.45747849623496,
1.42806953503212));
#23832=CARTESIAN_POINT('Ctrl Pts',(-0.638450508815834,1.41812713365384,
1.3646130604457));
#23833=CARTESIAN_POINT('Ctrl Pts',(-0.501744424014167,1.31319488582044,
1.2335702076553));
#23834=CARTESIAN_POINT('Ctrl Pts',(-0.45248307191557,1.25539949095026,1.17136442658356));
#23835=CARTESIAN_POINT('Ctrl Pts',(-0.414490807021284,1.19131159212569,
1.10727038327973));
#23836=CARTESIAN_POINT('Origin',(0.,0.,1.10727038327973));
#23837=CARTESIAN_POINT('Ctrl Pts',(-0.165188454748262,1.06503024383179,
1.28318567027397));
#23838=CARTESIAN_POINT('Ctrl Pts',(-0.246882731381371,1.27876982080874,
1.53751096017972));
#23839=CARTESIAN_POINT('Ctrl Pts',(-0.429465330327865,1.39803761752215,
1.74607168007008));
#23840=CARTESIAN_POINT('Ctrl Pts',(-0.712936251587744,1.42283363397204,
1.90886782994506));
#23841=CARTESIAN_POINT('Ctrl Pts',(-0.168932913531384,1.07930558594879,
1.26847940010162));
#23842=CARTESIAN_POINT('Ctrl Pts',(-0.252026844288351,1.29586765564979,
1.51987665322459));
#23843=CARTESIAN_POINT('Ctrl Pts',(-0.437225780288053,1.41640054440424,
1.72611612827485));
#23844=CARTESIAN_POINT('Ctrl Pts',(-0.724629310334697,1.44116225705855,
1.88704325648018));
#23845=CARTESIAN_POINT('Ctrl Pts',(-0.172580460092752,1.10652474870095,
1.24117906537517));
#23846=CARTESIAN_POINT('Ctrl Pts',(-0.257658341550684,1.32856177300788,
1.48716667186368));
#23847=CARTESIAN_POINT('Ctrl Pts',(-0.447493258920491,1.45233913898617,
1.68888789608761));
#23848=CARTESIAN_POINT('Ctrl Pts',(-0.742078309759816,1.47786361346603,
1.84634469876801));
#23849=CARTESIAN_POINT('Ctrl Pts',(-0.161305070542798,1.171005693206,1.18072695962337));
#23850=CARTESIAN_POINT('Ctrl Pts',(-0.246868029800147,1.40706779462019,
1.41461248446318));
#23851=CARTESIAN_POINT('Ctrl Pts',(-0.444855864337702,1.54132997390971,
1.60644654213684));
#23852=CARTESIAN_POINT('Ctrl Pts',(-0.755334809435783,1.57392460995617,
1.75614031701006));
#23853=CARTESIAN_POINT('Ctrl Pts',(-0.136821749681419,1.22396679065339,
1.13430117558029));
#23854=CARTESIAN_POINT('Ctrl Pts',(-0.21960593824905,1.47209169926767,1.35902160674437));
#23855=CARTESIAN_POINT('Ctrl Pts',(-0.422262554132523,1.61714699314179,
1.54332567193682));
#23856=CARTESIAN_POINT('Ctrl Pts',(-0.744733799933248,1.65939158627326,
1.68715809360678));
#23857=CARTESIAN_POINT('Ctrl Pts',(-0.114044962799315,1.26214347192869,
1.10192284729582));
#23858=CARTESIAN_POINT('Ctrl Pts',(-0.193861398098013,1.51913070253036,
1.32027771712106));
#23859=CARTESIAN_POINT('Ctrl Pts',(-0.399166585072151,1.67281935264038,
1.4993370241196));
#23860=CARTESIAN_POINT('Ctrl Pts',(-0.729960523721729,1.72320942225876,
1.63910076829144));
#23861=CARTESIAN_POINT('',(-0.166511139289342,1.06845992077163,1.28727233489076));
#23862=CARTESIAN_POINT('',(-0.117749801015222,1.25585067703094,1.10727038327973));
#23863=CARTESIAN_POINT('Ctrl Pts',(-0.166511139289342,1.06845992077163,
1.28727233489076));
#23864=CARTESIAN_POINT('Ctrl Pts',(-0.174823883464338,1.10004620708051,
1.25478273943433));
#23865=CARTESIAN_POINT('Ctrl Pts',(-0.172667519342151,1.12726776497775,
1.22829923781232));
#23866=CARTESIAN_POINT('Ctrl Pts',(-0.154814727716362,1.18657278434537,
1.17205963503373));
#23867=CARTESIAN_POINT('Ctrl Pts',(-0.14047414548886,1.21953445537415,1.14130666672595));
#23868=CARTESIAN_POINT('Ctrl Pts',(-0.117749801015222,1.25585067703094,
1.10727038327973));
#23869=CARTESIAN_POINT('Ctrl Pts',(-0.166511139289342,1.06845992077163,
1.28727233489076));
#23870=CARTESIAN_POINT('Ctrl Pts',(-0.203229920731113,1.16282366323453,
1.39987124007464));
#23871=CARTESIAN_POINT('Ctrl Pts',(-0.259800859583567,1.23859785430383,
1.50346488650363));
#23872=CARTESIAN_POINT('Ctrl Pts',(-0.431100013478375,1.36677481743678,
1.715480776583));
#23873=CARTESIAN_POINT('Ctrl Pts',(-0.556572568507924,1.40911659430226,
1.81902921434248));
#23874=CARTESIAN_POINT('Ctrl Pts',(-0.712641620935351,1.42280782457595,
1.90869858745619));
#23875=CARTESIAN_POINT('Ctrl Pts',(-0.117749801015222,1.25585067703094,
1.10727038327973));
#23876=CARTESIAN_POINT('Ctrl Pts',(-0.145300304395599,1.33766656151262,
1.18103565901044));
#23877=CARTESIAN_POINT('Ctrl Pts',(-0.18654898832971,1.41595401455117,1.25302429310889));
#23878=CARTESIAN_POINT('Ctrl Pts',(-0.30869349233915,1.55687787546591,1.39260788389877));
#23879=CARTESIAN_POINT('Ctrl Pts',(-0.387630019962927,1.61436582414941,
1.45574709063861));
#23880=CARTESIAN_POINT('Ctrl Pts',(-0.556523222076064,1.68758071271376,
1.55895701082589));
#23881=CARTESIAN_POINT('Ctrl Pts',(-0.636541741320461,1.70827005906903,
1.59904902099411));
#23882=CARTESIAN_POINT('Ctrl Pts',(-0.71964734468187,1.71930883511106,1.63615580822897));
#23883=CARTESIAN_POINT('Ctrl Pts',(-0.420870970491669,1.19577051030242,
1.1015723109602));
#23884=CARTESIAN_POINT('Ctrl Pts',(-0.561530328976122,1.425339146688,1.31988785480614));
#23885=CARTESIAN_POINT('Ctrl Pts',(-0.79847814597965,1.52384297854319,1.49890963328678));
#23886=CARTESIAN_POINT('Ctrl Pts',(-1.13171442150225,1.49128200586798,1.63863764640213));
#23887=CARTESIAN_POINT('Ctrl Pts',(-0.393355414961742,1.17679362500494,
1.12589971949673));
#23888=CARTESIAN_POINT('Ctrl Pts',(-0.527463617924698,1.40368256628313,
1.34900830339197));
#23889=CARTESIAN_POINT('Ctrl Pts',(-0.757891527007923,1.50373022520315,
1.53195557707744));
#23890=CARTESIAN_POINT('Ctrl Pts',(-1.08455939173712,1.47705841783302,1.67474624941237));
#23891=CARTESIAN_POINT('Ctrl Pts',(-0.352262141476107,1.14284817765567,
1.16769296545954));
#23892=CARTESIAN_POINT('Ctrl Pts',(-0.476355861470115,1.3645632700682,1.39903566442692));
#23893=CARTESIAN_POINT('Ctrl Pts',(-0.696074558068188,1.46622517664402,
1.58878359776798));
#23894=CARTESIAN_POINT('Ctrl Pts',(-1.01150165877891,1.44794881615932,1.73684050274469));
#23895=CARTESIAN_POINT('Ctrl Pts',(-0.308178085105591,1.09051150146367,
1.22804267083047));
#23896=CARTESIAN_POINT('Ctrl Pts',(-0.420725138053456,1.30325409768322,
1.47142154083508));
#23897=CARTESIAN_POINT('Ctrl Pts',(-0.626556636662153,1.40449154295595,
1.67099852964049));
#23898=CARTESIAN_POINT('Ctrl Pts',(-0.925684985930704,1.39421997501402,
1.8267672334207));
#23899=CARTESIAN_POINT('Ctrl Pts',(-0.295454942931511,1.05685857441837,
1.2635364344865));
#23900=CARTESIAN_POINT('Ctrl Pts',(-0.403825079433304,1.26316084408195,
1.51398418220584));
#23901=CARTESIAN_POINT('Ctrl Pts',(-0.602771168700623,1.36162184430235,
1.71946457116168));
#23902=CARTESIAN_POINT('Ctrl Pts',(-0.892463171324776,1.35249734632791,
1.87977332297457));
#23903=CARTESIAN_POINT('Ctrl Pts',(-0.292083537908477,1.03743092373275,
1.28318517919043));
#23904=CARTESIAN_POINT('Ctrl Pts',(-0.3989062505499,1.23982087453714,1.53754499301448));
#23905=CARTESIAN_POINT('Ctrl Pts',(-0.594546582101046,1.33626197576335,
1.74612783237291));
#23906=CARTESIAN_POINT('Ctrl Pts',(-0.879004532561914,1.32675422741137,
1.90893369726573));
#23907=CARTESIAN_POINT('',(-0.293809324770207,1.04067701160391,1.28727233489076));
#23908=CARTESIAN_POINT('Ctrl Pts',(-0.414490807021284,1.19131159212569,
1.10727038327973));
#23909=CARTESIAN_POINT('Ctrl Pts',(-0.393158028076679,1.17676901314191,
1.12801545944031));
#23910=CARTESIAN_POINT('Ctrl Pts',(-0.371002680489146,1.15945966570541,
1.15133239961407));
#23911=CARTESIAN_POINT('Ctrl Pts',(-0.335895470715533,1.124478707594,1.19509600545469));
#23912=CARTESIAN_POINT('Ctrl Pts',(-0.323050675538606,1.10930988332448,
1.21324740617417));
#23913=CARTESIAN_POINT('Ctrl Pts',(-0.305600782276718,1.08088339992881,
1.24538218411099));
#23914=CARTESIAN_POINT('Ctrl Pts',(-0.297892884779784,1.06407548086635,
1.26364457695016));
#23915=CARTESIAN_POINT('Ctrl Pts',(-0.293809324770207,1.04067701160391,
1.28727233489076));
#23916=CARTESIAN_POINT('Ctrl Pts',(-0.293809324770207,1.04067701160391,
1.28727233489076));
#23917=CARTESIAN_POINT('Ctrl Pts',(-0.341610972564374,1.12993947443311,
1.39987124007464));
#23918=CARTESIAN_POINT('Ctrl Pts',(-0.406884846288962,1.19835965101752,
1.50346488650363));
#23919=CARTESIAN_POINT('Ctrl Pts',(-0.592356746173702,1.30500348982786,
1.715480776583));
#23920=CARTESIAN_POINT('Ctrl Pts',(-0.722011051157661,1.33194693676576,
1.81902921434248));
#23921=CARTESIAN_POINT('Ctrl Pts',(-0.878593860895847,1.32676788217082,
1.90869858745619));
#23922=CARTESIAN_POINT('Ctrl Pts',(-0.293809324770207,1.04067701160391,
1.28727233489076));
#23923=CARTESIAN_POINT('Ctrl Pts',(-0.401287915254421,1.24137728305361,
1.54044292999952));
#23924=CARTESIAN_POINT('Ctrl Pts',(-0.59709613876759,1.3367108140079,1.74808806061869));
#23925=CARTESIAN_POINT('Ctrl Pts',(-0.881233995309716,1.32667760446677,
1.91020772674828));
#23926=CARTESIAN_POINT('Ctrl Pts',(-0.251376596276585,1.04993798132648,
1.28727233489076));
#23927=CARTESIAN_POINT('Ctrl Pts',(-0.35054884232117,1.25446154039629,1.54044292999952));
#23928=CARTESIAN_POINT('Ctrl Pts',(-0.542061247874906,1.35741454085596,
1.74808806061869));
#23929=CARTESIAN_POINT('Ctrl Pts',(-0.825913812937791,1.3587969827055,1.91020772674828));
#23930=CARTESIAN_POINT('Ctrl Pts',(-0.208943867782964,1.05919895104906,
1.28727233489076));
#23931=CARTESIAN_POINT('Ctrl Pts',(-0.299809769387921,1.26754579773896,
1.54044292999952));
#23932=CARTESIAN_POINT('Ctrl Pts',(-0.487026356982221,1.37811826770401,
1.74808806061869));
#23933=CARTESIAN_POINT('Ctrl Pts',(-0.770593630565866,1.39091636094422,
1.91020772674828));
#23934=CARTESIAN_POINT('Ctrl Pts',(-0.166511139289342,1.06845992077163,
1.28727233489076));
#23935=CARTESIAN_POINT('Ctrl Pts',(-0.24907069645467,1.28063005508163,1.54044292999952));
#23936=CARTESIAN_POINT('Ctrl Pts',(-0.431991466089537,1.39882199455207,
1.74808806061869));
#23937=CARTESIAN_POINT('Ctrl Pts',(-0.715273448193941,1.42303573918295,
1.91020772674828));
#23938=CARTESIAN_POINT('Ctrl Pts',(-0.293809324770207,1.04067701160391,
1.28727233489076));
#23939=CARTESIAN_POINT('Ctrl Pts',(-0.272797358647504,1.04588229398058,
1.28797191329047));
#23940=CARTESIAN_POINT('Ctrl Pts',(-0.251713870469976,1.05079925066492,
1.28831907556383));
#23941=CARTESIAN_POINT('Ctrl Pts',(-0.230554570986284,1.05542144523633,
1.288319084765));
#23942=CARTESIAN_POINT('Ctrl Pts',(-0.209262869938631,1.06007256258898,
1.28831909402374));
#23943=CARTESIAN_POINT('Ctrl Pts',(-0.187915901626935,1.06442048323406,
1.28796761487395));
#23944=CARTESIAN_POINT('Ctrl Pts',(-0.166511139289342,1.06845992077163,
1.28727233489076));
#23945=CARTESIAN_POINT('Origin',(0.,0.,1.37171309575435));
#23946=CARTESIAN_POINT('',(-0.0260686553993153,1.26108935601086,1.10727038327973));
#23947=CARTESIAN_POINT('Ctrl Pts',(-0.602229799711917,1.76386916735272,
1.63615580822897));
#23948=CARTESIAN_POINT('Ctrl Pts',(-0.497389884697211,1.74092498377319,
1.58735805514609));
#23949=CARTESIAN_POINT('Ctrl Pts',(-0.406388294299314,1.70624968855532,
1.53858095020837));
#23950=CARTESIAN_POINT('Ctrl Pts',(-0.240766166368975,1.61071325107043,
1.42806953503213));
#23951=CARTESIAN_POINT('Ctrl Pts',(-0.168977132257998,1.54601110868789,
1.36461306044571));
#23952=CARTESIAN_POINT('Ctrl Pts',(-0.0713877673286501,1.40397010717826,
1.23357020765531));
#23953=CARTESIAN_POINT('Ctrl Pts',(-0.0423971966252646,1.33378082531076,
1.17136442658356));
#23954=CARTESIAN_POINT('Ctrl Pts',(-0.0260686553993154,1.26108935601086,
1.10727038327973));
#23955=CARTESIAN_POINT('Origin',(0.,0.,1.10727038327973));
#23956=CARTESIAN_POINT('Ctrl Pts',(0.172008888562255,1.06394999323939,1.28318567027397));
#23957=CARTESIAN_POINT('Ctrl Pts',(0.160362439116273,1.2924681694826,1.53750521640541));
#23958=CARTESIAN_POINT('Ctrl Pts',(0.0235777602513121,1.46231719972917,
1.74606225962531));
#23959=CARTESIAN_POINT('Ctrl Pts',(-0.238345148032627,1.57349708397912,
1.90885679993368));
#23960=CARTESIAN_POINT('Ctrl Pts',(0.172859187306825,1.07868665224636,1.2684765050474));
#23961=CARTESIAN_POINT('Ctrl Pts',(0.160753683145647,1.31032224774096,1.51986749395221));
#23962=CARTESIAN_POINT('Ctrl Pts',(0.0218713714335433,1.48218332835239,
1.72610289246662));
#23963=CARTESIAN_POINT('Ctrl Pts',(-0.243802874063088,1.59454606057878,
1.8870280554852));
#23964=CARTESIAN_POINT('Ctrl Pts',(0.177804687773572,1.10570688269946,1.24116976953012));
#23965=CARTESIAN_POINT('Ctrl Pts',(0.16550438356704,1.34316347164223,1.48715026946299));
#23966=CARTESIAN_POINT('Ctrl Pts',(0.0232152493262187,1.51954478212276,
1.68886609246491));
#23967=CARTESIAN_POINT('Ctrl Pts',(-0.249054092840224,1.63485294054343,
1.84632034153071));
#23968=CARTESIAN_POINT('Ctrl Pts',(0.208466906889381,1.16355954955659,1.18070453025513));
#23969=CARTESIAN_POINT('Ctrl Pts',(0.200040954183214,1.41450709648089,1.41458088343679));
#23970=CARTESIAN_POINT('Ctrl Pts',(0.0532384711777704,1.60338349810865,
1.60640735029516));
#23971=CARTESIAN_POINT('Ctrl Pts',(-0.231963472934463,1.73033051533549,
1.75609715466375));
#23972=CARTESIAN_POINT('Ctrl Pts',(0.248125754775117,1.20636749722078,1.13427327868628));
#23973=CARTESIAN_POINT('Ctrl Pts',(0.246072078233561,1.46793051395096,1.35898312394783));
#23974=CARTESIAN_POINT('Ctrl Pts',(0.0981648464084913,1.6685146591454,1.54327941073123));
#23975=CARTESIAN_POINT('Ctrl Pts',(-0.195461051586314,1.80834818125255,
1.6871068853877));
#23976=CARTESIAN_POINT('Ctrl Pts',(0.281595159362692,1.235641855012,1.10188938448118));
#23977=CARTESIAN_POINT('Ctrl Pts',(0.285104353628413,1.50471757474417,1.32023273220193));
#23978=CARTESIAN_POINT('Ctrl Pts',(0.137346783688563,1.71433282083683,1.49928348142626));
#23979=CARTESIAN_POINT('Ctrl Pts',(-0.161677550456858,1.86448759328998,
1.63904163215416));
#23980=CARTESIAN_POINT('',(0.171810769270086,1.06762054184321,1.28727233489076));
#23981=CARTESIAN_POINT('',(0.27609248605186,1.23077165948193,1.10727038327973));
#23982=CARTESIAN_POINT('Ctrl Pts',(0.171810769270086,1.06762054184321,1.28727233489076));
#23983=CARTESIAN_POINT('Ctrl Pts',(0.173665579012839,1.10022966448354,1.25478273943359));
#23984=CARTESIAN_POINT('Ctrl Pts',(0.184128327166778,1.12545255134546,1.22829923781164));
#23985=CARTESIAN_POINT('Ctrl Pts',(0.219433599813404,1.17633816045551,1.17205963503211));
#23986=CARTESIAN_POINT('Ctrl Pts',(0.243258020499799,1.20325508885771,1.14130666672433));
#23987=CARTESIAN_POINT('Ctrl Pts',(0.27609248605186,1.23077165948193,1.10727038327973));
#23988=CARTESIAN_POINT('Ctrl Pts',(0.171810769270086,1.06762054184321,1.28727233489076));
#23989=CARTESIAN_POINT('Ctrl Pts',(0.166049132983329,1.16871252149279,1.39987124007464));
#23990=CARTESIAN_POINT('Ctrl Pts',(0.135662485730195,1.2582594411694,1.50346488650363));
#23991=CARTESIAN_POINT('Ctrl Pts',(0.012356169078144,1.43309732687145,1.715480776583));
#23992=CARTESIAN_POINT('Ctrl Pts',(-0.093890993375447,1.51213990150266,
1.81902921434248));
#23993=CARTESIAN_POINT('Ctrl Pts',(-0.238090659850087,1.57338902476662,
1.90869858745619));
#23994=CARTESIAN_POINT('Ctrl Pts',(0.27609248605186,1.23077165948193,1.10727038327973));
#23995=CARTESIAN_POINT('Ctrl Pts',(0.275172898999398,1.31709676330282,1.18103565901045));
#23996=CARTESIAN_POINT('Ctrl Pts',(0.260135222790497,1.40429909999054,1.25302429310892));
#23997=CARTESIAN_POINT('Ctrl Pts',(0.18956320279641,1.57122974978699,1.38867432147871));
#23998=CARTESIAN_POINT('Ctrl Pts',(0.136388204217674,1.64657149028481,1.44891114041819));
#23999=CARTESIAN_POINT('Ctrl Pts',(0.00179051121351582,1.7707701091784,
1.55340617058601));
#24000=CARTESIAN_POINT('Ctrl Pts',(-0.0722162251277863,1.8188345687539,
1.59645518670947));
#24001=CARTESIAN_POINT('Ctrl Pts',(-0.153129647965885,1.85754313061971,
1.63615580822897));
#24002=CARTESIAN_POINT('Ctrl Pts',(-0.0307586699497086,1.2673016181377,
1.10157231096021));
#24003=CARTESIAN_POINT('Ctrl Pts',(-0.0935930593956182,1.52910049789877,
1.31988785480615));
#24004=CARTESIAN_POINT('Ctrl Pts',(-0.288504466724439,1.69600411129883,
1.4989096332868));
#24005=CARTESIAN_POINT('Ctrl Pts',(-0.615492891936171,1.76801245833786,
1.63863764640215));
#24006=CARTESIAN_POINT('Ctrl Pts',(-0.0104540016207206,1.24075075344812,
1.12589971949673));
#24007=CARTESIAN_POINT('Ctrl Pts',(-0.067885943246571,1.49797667332671,
1.34900830339198));
#24008=CARTESIAN_POINT('Ctrl Pts',(-0.256119480862732,1.66433379116766,
1.53195557707745));
#24009=CARTESIAN_POINT('Ctrl Pts',(-0.575041124025735,1.73991331668443,
1.67474624941239));
#24010=CARTESIAN_POINT('Ctrl Pts',(0.0181391694102201,1.19576910668283,
1.16769197379075));
#24011=CARTESIAN_POINT('Ctrl Pts',(-0.0313672401565047,1.44497975845611,
1.39903467275813));
#24012=CARTESIAN_POINT('Ctrl Pts',(-0.208916886053927,1.60956344041243,
1.58878224232001));
#24013=CARTESIAN_POINT('Ctrl Pts',(-0.514553591586059,1.68965392328533,
1.73683914729673));
#24014=CARTESIAN_POINT('Ctrl Pts',(0.0438923944102215,1.13237144427268,
1.22804151155252));
#24015=CARTESIAN_POINT('Ctrl Pts',(0.00259486397362439,1.36948062872854,
1.47142038155714));
#24016=CARTESIAN_POINT('Ctrl Pts',(-0.161878639424906,1.52936917527703,
1.67099694623232));
#24017=CARTESIAN_POINT('Ctrl Pts',(-0.449540694258325,1.61203607707659,
1.82676565001253));
#24018=CARTESIAN_POINT('Ctrl Pts',(0.0455929113995307,1.09643283244092,
1.2635364344865));
#24019=CARTESIAN_POINT('Ctrl Pts',(0.00627769421187257,1.32612616419273,
1.51398418220584));
#24020=CARTESIAN_POINT('Ctrl Pts',(-0.152505158025998,1.48124586260132,
1.71946457116169));
#24021=CARTESIAN_POINT('Ctrl Pts',(-0.430838249779549,1.56208770129018,
1.87977332297459));
#24022=CARTESIAN_POINT('Ctrl Pts',(0.0427958338931189,1.07691421721301,
1.28318517919043));
#24023=CARTESIAN_POINT('Ctrl Pts',(0.00374333123643569,1.30240853234962,
1.53754499301448));
#24024=CARTESIAN_POINT('Ctrl Pts',(-0.152519741700302,1.45458565734394,
1.74612783237292));
#24025=CARTESIAN_POINT('Ctrl Pts',(-0.425993384917093,1.53344559219597,
1.90893369726574));
#24026=CARTESIAN_POINT('',(0.042157609369957,1.08053472770428,1.28727233489076));
#24027=CARTESIAN_POINT('Ctrl Pts',(-0.0260686553993156,1.26108935601086,
1.10727038327973));
#24028=CARTESIAN_POINT('Ctrl Pts',(-0.0102738810212675,1.2406663502733,
1.12801545944048));
#24029=CARTESIAN_POINT('Ctrl Pts',(0.00544822415320251,1.21735780368012,
1.15133239961429));
#24030=CARTESIAN_POINT('Ctrl Pts',(0.0280274542413815,1.17324021107692,
1.19509600545487));
#24031=CARTESIAN_POINT('Ctrl Pts',(0.0355561559109005,1.15484454191172,
1.21324740617454));
#24032=CARTESIAN_POINT('Ctrl Pts',(0.0433677241466949,1.12241703607498,
1.24538218411135));
#24033=CARTESIAN_POINT('Ctrl Pts',(0.0455044376575714,1.10404988380783,
1.26364457695051));
#24034=CARTESIAN_POINT('Ctrl Pts',(0.042157609369957,1.08053472770428,1.28727233489076));
#24035=CARTESIAN_POINT('Ctrl Pts',(0.042157609369957,1.08053472770428,1.28727233489076));
#24036=CARTESIAN_POINT('Ctrl Pts',(0.0242791587196549,1.18019989616608,
1.39987124007464));
#24037=CARTESIAN_POINT('Ctrl Pts',(-0.0166569869072257,1.26544208722232,
1.50346488650363));
#24038=CARTESIAN_POINT('Ctrl Pts',(-0.16009648734447,1.42418037408903,1.715480776583));
#24039=CARTESIAN_POINT('Ctrl Pts',(-0.275079075974333,1.48987049850469,
1.81902921434248));
#24040=CARTESIAN_POINT('Ctrl Pts',(-0.425598593400271,1.53333167412,1.90869858745619));
#24041=CARTESIAN_POINT('Ctrl Pts',(0.042157609369957,1.08053472770428,1.28727233489076));
#24042=CARTESIAN_POINT('Ctrl Pts',(0.00195919018135101,1.30462473967982,
1.54044292999952));
#24043=CARTESIAN_POINT('Ctrl Pts',(-0.154805815536382,1.45580038421926,
1.74808806061869));
#24044=CARTESIAN_POINT('Ctrl Pts',(-0.428137407783241,1.5340616613226,1.91020772674828));
#24045=CARTESIAN_POINT('Ctrl Pts',(0.0853753293366667,1.07622999908393,
1.28727233489076));
#24046=CARTESIAN_POINT('Ctrl Pts',(0.0542581740029553,1.30138937207125,
1.54044292999952));
#24047=CARTESIAN_POINT('Ctrl Pts',(-0.0960667204863544,1.45848408198029,
1.74808806061869));
#24048=CARTESIAN_POINT('Ctrl Pts',(-0.365599354131263,1.54751412881105,
1.91020772674828));
#24049=CARTESIAN_POINT('Ctrl Pts',(0.128593049303376,1.07192527046357,1.28727233489076));
#24050=CARTESIAN_POINT('Ctrl Pts',(0.106557157824559,1.29815400446268,1.54044292999952));
#24051=CARTESIAN_POINT('Ctrl Pts',(-0.0373276254363276,1.46116777974132,
1.74808806061869));
#24052=CARTESIAN_POINT('Ctrl Pts',(-0.303061300479284,1.56096659629949,
1.91020772674828));
#24053=CARTESIAN_POINT('Ctrl Pts',(0.171810769270086,1.06762054184321,1.28727233489076));
#24054=CARTESIAN_POINT('Ctrl Pts',(0.158856141646164,1.29491863685411,1.54044292999952));
#24055=CARTESIAN_POINT('Ctrl Pts',(0.0214114696136998,1.46385147750235,
1.74808806061869));
#24056=CARTESIAN_POINT('Ctrl Pts',(-0.240523246827306,1.57441906378793,
1.91020772674828));
#24057=CARTESIAN_POINT('Ctrl Pts',(0.042157609369957,1.08053472770428,1.28727233489076));
#24058=CARTESIAN_POINT('Ctrl Pts',(0.0637496973860413,1.07899219081063,
1.28797191329047));
#24059=CARTESIAN_POINT('Ctrl Pts',(0.0853207093795777,1.07715333835806,
1.28831907556383));
#24060=CARTESIAN_POINT('Ctrl Pts',(0.106872735707655,1.07501072349525,1.288319084765));
#24061=CARTESIAN_POINT('Ctrl Pts',(0.128559621036836,1.07285470149866,1.28831909402374));
#24062=CARTESIAN_POINT('Ctrl Pts',(0.150205375722349,1.07039324377381,1.28796761487395));
#24063=CARTESIAN_POINT('Ctrl Pts',(0.171810769270086,1.06762054184321,1.28727233489076));
#24064=CARTESIAN_POINT('Origin',(0.,0.,1.37171309575435));
#24065=CARTESIAN_POINT('',(0.364905277844141,1.20742290720348,1.10727038327973));
#24066=CARTESIAN_POINT('Ctrl Pts',(-0.0276890267571662,1.86363850813291,
1.63615580822897));
#24067=CARTESIAN_POINT('Ctrl Pts',(0.0698239366988456,1.80655480211405,
1.5847793405579));
#24068=CARTESIAN_POINT('Ctrl Pts',(0.148691945288455,1.74187241700965,1.53343685544661));
#24069=CARTESIAN_POINT('Ctrl Pts',(0.274785130849249,1.59669345888594,1.42076782591243));
#24070=CARTESIAN_POINT('Ctrl Pts',(0.320436333138568,1.51444831269989,1.3583029222602));
#24071=CARTESIAN_POINT('Ctrl Pts',(0.36627106501613,1.35321270714143,1.23020598103185));
#24072=CARTESIAN_POINT('Ctrl Pts',(0.371649422530895,1.27957619027631,1.16961370091491));
#24073=CARTESIAN_POINT('Ctrl Pts',(0.364905277844141,1.20742290720348,1.10727038327973));
#24074=CARTESIAN_POINT('Origin',(0.,0.,1.10727038327973));
#24075=CARTESIAN_POINT('Ctrl Pts',(0.492368803403902,0.958722904333223,
1.28318567027397));
#24076=CARTESIAN_POINT('Ctrl Pts',(0.551909716442827,1.17966054547972,1.53751096017971));
#24077=CARTESIAN_POINT('Ctrl Pts',(0.47430114299954,1.3834695788885,1.74607168007007));
#24078=CARTESIAN_POINT('Ctrl Pts',(0.259543083074042,1.57015000455957,1.90886782994504));
#24079=CARTESIAN_POINT('Ctrl Pts',(0.497730308181424,0.97247283635693,1.26847940010162));
#24080=CARTESIAN_POINT('Ctrl Pts',(0.557797896845798,1.19651661813599,1.51987665322458));
#24081=CARTESIAN_POINT('Ctrl Pts',(0.47881626470797,1.40288697684033,1.72611612827483));
#24082=CARTESIAN_POINT('Ctrl Pts',(0.260856494176611,1.5918511796057,1.88704325648016));
#24083=CARTESIAN_POINT('Ctrl Pts',(0.510779460904231,0.996638068239397,
1.24117819097188));
#24084=CARTESIAN_POINT('Ctrl Pts',(0.572460097309863,1.2262773183014,1.48716579746039));
#24085=CARTESIAN_POINT('Ctrl Pts',(0.491635127338188,1.43799804358594,1.68888670640877));
#24086=CARTESIAN_POINT('Ctrl Pts',(0.268313724592168,1.63180052564182,1.84634350908917));
#24087=CARTESIAN_POINT('Ctrl Pts',(0.557803663431837,1.04217697649276,1.18072535874296));
#24088=CARTESIAN_POINT('Ctrl Pts',(0.627335597140059,1.28344787385866,1.41461088358276));
#24089=CARTESIAN_POINT('Ctrl Pts',(0.546077997260116,1.50844372983685,1.60644436926605));
#24090=CARTESIAN_POINT('Ctrl Pts',(0.314053900652136,1.71730828939987,1.75613814413928));
#24091=CARTESIAN_POINT('Ctrl Pts',(0.608738508149429,1.07063174084475,1.13430117558029));
#24092=CARTESIAN_POINT('Ctrl Pts',(0.687608854742563,1.32002833380447,1.35902160674437));
#24093=CARTESIAN_POINT('Ctrl Pts',(0.60891757097649,1.55649910176849,1.54332567193681));
#24094=CARTESIAN_POINT('Ctrl Pts',(0.372863601758246,1.78021953810235,1.68715809360677));
#24095=CARTESIAN_POINT('Ctrl Pts',(0.649605006049397,1.08812946536139,1.10192284729582));
#24096=CARTESIAN_POINT('Ctrl Pts',(0.736085457637466,1.34295142581461,1.32027771712105));
#24097=CARTESIAN_POINT('Ctrl Pts',(0.660325994321484,1.58796351671871,1.49933702411959));
#24098=CARTESIAN_POINT('Ctrl Pts',(0.422326616101449,1.82316573807366,1.63910076829142));
#24099=CARTESIAN_POINT('',(0.493314642657339,0.962275025729455,1.28727233489076));
#24100=CARTESIAN_POINT('',(0.642908916934723,1.08521613661244,1.10727038327973));
#24101=CARTESIAN_POINT('Ctrl Pts',(0.493314642657339,0.962275025729455,
1.28727233489076));
#24102=CARTESIAN_POINT('Ctrl Pts',(0.505155444617114,0.992714976575168,
1.2547827394338));
#24103=CARTESIAN_POINT('Ctrl Pts',(0.522900410114692,1.01347020049763,1.22829923781183));
#24104=CARTESIAN_POINT('Ctrl Pts',(0.572202237707941,1.0509553613877,1.17205963503352));
#24105=CARTESIAN_POINT('Ctrl Pts',(0.603178396560795,1.06919273067027,1.14130666672584));
#24106=CARTESIAN_POINT('Ctrl Pts',(0.642908916934723,1.08521613661244,1.10727038327973));
#24107=CARTESIAN_POINT('Ctrl Pts',(0.493314642657339,0.962275025729455,
1.28727233489076));
#24108=CARTESIAN_POINT('Ctrl Pts',(0.519074140629024,1.06019965524839,1.39987124007464));
#24109=CARTESIAN_POINT('Ctrl Pts',(0.517846241724568,1.15475382712427,1.50346488650363));
#24110=CARTESIAN_POINT('Ctrl Pts',(0.454602843714802,1.35913828497575,1.715480776583));
#24111=CARTESIAN_POINT('Ctrl Pts',(0.377981286365637,1.46714441944577,1.81902921434248));
#24112=CARTESIAN_POINT('Ctrl Pts',(0.259766273896474,1.5699559447672,1.90869858745619));
#24113=CARTESIAN_POINT('Ctrl Pts',(0.642908916934723,1.08521613661244,1.10727038327973));
#24114=CARTESIAN_POINT('Ctrl Pts',(0.668710261798007,1.16760035714814,1.18103565901043));
#24115=CARTESIAN_POINT('Ctrl Pts',(0.681355585835306,1.25518160519559,1.25302429310887));
#24116=CARTESIAN_POINT('Ctrl Pts',(0.665371573463983,1.44098614169386,1.39260788389875));
#24117=CARTESIAN_POINT('Ctrl Pts',(0.635301149560116,1.533892595955,1.45574709063858));
#24118=CARTESIAN_POINT('Ctrl Pts',(0.54169831056255,1.6923976184594,1.55895701082588));
#24119=CARTESIAN_POINT('Ctrl Pts',(0.489122861296305,1.75616935678547,1.5990490209941));
#24120=CARTESIAN_POINT('Ctrl Pts',(0.428377445609995,1.81394816223928,1.63615580822897));
#24121=CARTESIAN_POINT('Ctrl Pts',(0.362330138275325,1.21487793679796,1.10149705943222));
#24122=CARTESIAN_POINT('Ctrl Pts',(0.383459937582895,1.48329895916361,1.31979778023781));
#24123=CARTESIAN_POINT('Ctrl Pts',(0.24964496094192,1.70227260218965,1.49880741124997));
#24124=CARTESIAN_POINT('Ctrl Pts',(-0.0391147916476021,1.8717988658761,
1.63852595246867));
#24125=CARTESIAN_POINT('Ctrl Pts',(0.373447482460586,1.18333690797345,1.12583385309083));
#24126=CARTESIAN_POINT('Ctrl Pts',(0.398305182537801,1.44573672483851,1.34892944774502));
#24127=CARTESIAN_POINT('Ctrl Pts',(0.270675994878907,1.66212671668266,1.5318660237053));
#24128=CARTESIAN_POINT('Ctrl Pts',(-0.00930365130124667,1.83255854794258,
1.67464838892921));
#24129=CARTESIAN_POINT('Ctrl Pts',(0.386758017000779,1.13169790455625,1.16764044916317));
#24130=CARTESIAN_POINT('Ctrl Pts',(0.416680587119747,1.38402127269754,1.39897336709084));
#24131=CARTESIAN_POINT('Ctrl Pts',(0.298670375694659,1.59542335194444,1.58871211231352));
#24132=CARTESIAN_POINT('Ctrl Pts',(0.0327265383253287,1.76604232095016,
1.73676275687621));
#24133=CARTESIAN_POINT('Ctrl Pts',(0.391671741837559,1.06341115236232,1.22801607619329));
#24134=CARTESIAN_POINT('Ctrl Pts',(0.425665904909546,1.30168216224369,1.47139032317727));
#24135=CARTESIAN_POINT('Ctrl Pts',(0.318647566754322,1.50457544636211,1.67096220367119));
#24136=CARTESIAN_POINT('Ctrl Pts',(0.0706042875438467,1.67209124376878,
1.82672793765153));
#24137=CARTESIAN_POINT('Ctrl Pts',(0.38218165487343,1.0286884268729,1.263527751515));
#24138=CARTESIAN_POINT('Ctrl Pts',(0.415770412604395,1.25929056133869,1.51397381108002));
#24139=CARTESIAN_POINT('Ctrl Pts',(0.312692596804323,1.45588630034146,1.71945276482244));
#24140=CARTESIAN_POINT('Ctrl Pts',(0.0729619965738786,1.61878272768801,
1.8797604367197));
#24141=CARTESIAN_POINT('Ctrl Pts',(0.373486051297297,1.01098164381094,1.28318517919159));
#24142=CARTESIAN_POINT('Ctrl Pts',(0.40602648967972,1.23750736860246,1.53754499301511));
#24143=CARTESIAN_POINT('Ctrl Pts',(0.304436793685255,1.43052436008973,1.74612783237316));
#24144=CARTESIAN_POINT('Ctrl Pts',(0.0687169633139001,1.59003261827273,
1.90893369726573));
#24145=CARTESIAN_POINT('',(0.373997862975654,1.01462217612883,1.28727233489076));
#24146=CARTESIAN_POINT('Ctrl Pts',(0.364905277844141,1.20742290720348,1.10727038327973));
#24147=CARTESIAN_POINT('Ctrl Pts',(0.373615945090653,1.18311862080936,1.12801545944044));
#24148=CARTESIAN_POINT('Ctrl Pts',(0.381365818655247,1.15609247800031,1.15133239961422));
#24149=CARTESIAN_POINT('Ctrl Pts',(0.389206856698251,1.10715678825455,1.19509600545488));
#24150=CARTESIAN_POINT('Ctrl Pts',(0.390682503085348,1.08733497046199,1.21324740617447));
#24151=CARTESIAN_POINT('Ctrl Pts',(0.388091095569742,1.05408067239124,1.24538218411122));
#24152=CARTESIAN_POINT('Ctrl Pts',(0.384447468688942,1.03595219175479,1.26364457695038));
#24153=CARTESIAN_POINT('Ctrl Pts',(0.373997862975654,1.01462217612883,1.28727233489076));
#24154=CARTESIAN_POINT('Ctrl Pts',(0.373997862975654,1.01462217612883,1.28727233489076));
#24155=CARTESIAN_POINT('Ctrl Pts',(0.387792676785359,1.11493412912611,1.39987124007464));
#24156=CARTESIAN_POINT('Ctrl Pts',(0.375201374409042,1.20865423507634,1.50346488650363));
#24157=CARTESIAN_POINT('Ctrl Pts',(0.287835131123856,1.40394856048621,1.715480776583));
#24158=CARTESIAN_POINT('Ctrl Pts',(0.198779555753984,1.50195515531182,1.81902921434248));
#24159=CARTESIAN_POINT('Ctrl Pts',(0.0690572297370888,1.58980227845634,
1.90869858745619));
#24160=CARTESIAN_POINT('Ctrl Pts',(0.373997862975653,1.01462217612883,1.28727233489076));
#24161=CARTESIAN_POINT('Ctrl Pts',(0.405014516431692,1.24016643693111,1.54044292999952));
#24162=CARTESIAN_POINT('Ctrl Pts',(0.302637979515068,1.43238606966553,1.74808806061869));
#24163=CARTESIAN_POINT('Ctrl Pts',(0.0668682522257825,1.59128107433209,
1.91020772674828));
#24164=CARTESIAN_POINT('Ctrl Pts',(0.413770122869549,0.997173125995706,
1.28727233489076));
#24165=CARTESIAN_POINT('Ctrl Pts',(0.453754022216744,1.22092814469495,1.54044292999952));
#24166=CARTESIAN_POINT('Ctrl Pts',(0.359331486839601,1.41678703930426,1.74808806061869));
#24167=CARTESIAN_POINT('Ctrl Pts',(0.130502516738118,1.58474980982363,1.91020772674828));
#24168=CARTESIAN_POINT('Ctrl Pts',(0.453542382763444,0.97972407586258,1.28727233489076));
#24169=CARTESIAN_POINT('Ctrl Pts',(0.502493528001797,1.2016898524588,1.54044292999952));
#24170=CARTESIAN_POINT('Ctrl Pts',(0.416024994164134,1.40118800894299,1.74808806061869));
#24171=CARTESIAN_POINT('Ctrl Pts',(0.194136781250454,1.57821854531517,1.91020772674828));
#24172=CARTESIAN_POINT('Ctrl Pts',(0.493314642657339,0.962275025729455,
1.28727233489076));
#24173=CARTESIAN_POINT('Ctrl Pts',(0.55123303378685,1.18245156022264,1.54044292999952));
#24174=CARTESIAN_POINT('Ctrl Pts',(0.472718501488667,1.38558897858172,1.74808806061869));
#24175=CARTESIAN_POINT('Ctrl Pts',(0.257771045762789,1.5716872808067,1.91020772674828));
#24176=CARTESIAN_POINT('Ctrl Pts',(0.373997862975653,1.01462217612883,1.28727233489076));
#24177=CARTESIAN_POINT('Ctrl Pts',(0.394056488869171,1.00648281422349,1.28797191329047));
#24178=CARTESIAN_POINT('Ctrl Pts',(0.414003503730716,0.998068152324094,
1.28831907556383));
#24179=CARTESIAN_POINT('Ctrl Pts',(0.433838594404394,0.989370462098314,
1.288319084765));
#24180=CARTESIAN_POINT('Ctrl Pts',(0.453797800577664,0.980618347207408,
1.28831909402374));
#24181=CARTESIAN_POINT('Ctrl Pts',(0.473623504353529,0.971588455744707,
1.28796761487395));
#24182=CARTESIAN_POINT('Ctrl Pts',(0.493314642657339,0.962275025729455,
1.28727233489076));
#24183=CARTESIAN_POINT('Origin',(0.,0.,1.37171309575435));
#24184=CARTESIAN_POINT('',(0.720159740047642,1.03556549162895,1.10727038327973));
#24185=CARTESIAN_POINT('Ctrl Pts',(0.549562141057369,1.78098192700405,1.63615580822897));
#24186=CARTESIAN_POINT('Ctrl Pts',(0.620893161259242,1.70079633666882,1.58735805514603));
#24187=CARTESIAN_POINT('Ctrl Pts',(0.674133367258296,1.61925404078154,1.53858095020831));
#24188=CARTESIAN_POINT('Ctrl Pts',(0.751969574388259,1.44461319502357,1.42806953503212));
#24189=CARTESIAN_POINT('Ctrl Pts',(0.772017157909613,1.35007152673687,1.3646130604457));
#24190=CARTESIAN_POINT('Ctrl Pts',(0.767479006699498,1.17779635313149,1.23357020765531));
#24191=CARTESIAN_POINT('Ctrl Pts',(0.749676646324452,1.10397180136272,1.17136442658356));
#24192=CARTESIAN_POINT('Ctrl Pts',(0.720159740047642,1.03556549162895,1.10727038327973));
#24193=CARTESIAN_POINT('Origin',(0.,0.,1.10727038327973));
#24194=CARTESIAN_POINT('Ctrl Pts',(0.764532229233201,0.759649337735664,
1.28318567027397));
#24195=CARTESIAN_POINT('Ctrl Pts',(0.889432488376415,0.951374367053291,
1.53751096017971));
#24196=CARTESIAN_POINT('Ctrl Pts',(0.87860280381325,1.1691906444597,1.74607168007007));
#24197=CARTESIAN_POINT('Ctrl Pts',(0.732043175543707,1.4130981699549,1.90886782994504));
#24198=CARTESIAN_POINT('Ctrl Pts',(0.773880285955837,0.771069504093749,
1.26847940010162));
#24199=CARTESIAN_POINT('Ctrl Pts',(0.90024129362699,0.965585896981722,1.51987665322458));
#24200=CARTESIAN_POINT('Ctrl Pts',(0.888897245689574,1.18626243797171,1.72611612827484));
#24201=CARTESIAN_POINT('Ctrl Pts',(0.739998335618541,1.43333134754249,1.88704325648016));
#24202=CARTESIAN_POINT('Ctrl Pts',(0.793756470105422,0.790019380359273,
1.24117952306876));
#24203=CARTESIAN_POINT('Ctrl Pts',(0.923380672132907,0.989358920654668,
1.48716712955727));
#24204=CARTESIAN_POINT('Ctrl Pts',(0.911936310735741,1.2156928538318,1.68888851879237));
#24205=CARTESIAN_POINT('Ctrl Pts',(0.759433295933273,1.46902007592139,1.84634532147277));
#24206=CARTESIAN_POINT('Ctrl Pts',(0.852549487780079,0.818798433422949,
1.18072779772815));
#24207=CARTESIAN_POINT('Ctrl Pts',(0.993235093958044,1.02677414338758,1.41461332256794));
#24208=CARTESIAN_POINT('Ctrl Pts',(0.985480669746799,1.26586652272337,1.60644767971084));
#24209=CARTESIAN_POINT('Ctrl Pts',(0.829355339157893,1.53620791207526,1.75614145458407));
#24210=CARTESIAN_POINT('Ctrl Pts',(0.909788127533563,0.830120749534194,
1.13430117558029));
#24211=CARTESIAN_POINT('Ctrl Pts',(1.06186607016719,1.04293872696083,1.35902160674436));
#24212=CARTESIAN_POINT('Ctrl Pts',(1.06009969793962,1.29215273573923,1.54332567193682));
#24213=CARTESIAN_POINT('Ctrl Pts',(0.904732449133408,1.57786820262104,1.68715809360678));
#24214=CARTESIAN_POINT('Ctrl Pts',(0.954061570898026,0.834133632104406,
1.10192284729582));
#24215=CARTESIAN_POINT('Ctrl Pts',(1.115053684233,1.04975978886662,1.32027771712105));
#24216=CARTESIAN_POINT('Ctrl Pts',(1.11871505289201,1.30619109614142,1.49933702411959));
#24217=CARTESIAN_POINT('Ctrl Pts',(0.965045676875069,1.60342755392881,1.63910076829143));
#24218=CARTESIAN_POINT('',(0.766529441696069,0.762735325532963,1.28727233489076));
#24219=CARTESIAN_POINT('',(0.946792943618195,0.833432097145889,1.10727038327973));
#24220=CARTESIAN_POINT('Ctrl Pts',(0.766529441696069,0.762735325532963,
1.28727233489076));
#24221=CARTESIAN_POINT('Ctrl Pts',(0.787197175677519,0.788026430108106,
1.25478273943352));
#24222=CARTESIAN_POINT('Ctrl Pts',(0.81048735765961,0.8022823251633,1.22829923781154));
#24223=CARTESIAN_POINT('Ctrl Pts',(0.868959733809894,0.822697729112222,
1.17205963503275));
#24224=CARTESIAN_POINT('Ctrl Pts',(0.904055468577541,0.830470338502301,
1.14130666672531));
#24225=CARTESIAN_POINT('Ctrl Pts',(0.946792943618196,0.833432097145889,
1.10727038327973));
#24226=CARTESIAN_POINT('Ctrl Pts',(0.766529441696069,0.762735325532963,
1.28727233489076));
#24227=CARTESIAN_POINT('Ctrl Pts',(0.821288554787752,0.847907059902912,
1.39987124007464));
#24228=CARTESIAN_POINT('Ctrl Pts',(0.849339599532016,0.938212862837218,
1.50346488650363));
#24229=CARTESIAN_POINT('Ctrl Pts',(0.852349824604395,1.15213731807335,1.715480776583));
#24230=CARTESIAN_POINT('Ctrl Pts',(0.812854124246773,1.27853461941729,1.81902921434248));
#24231=CARTESIAN_POINT('Ctrl Pts',(0.732195474855993,1.41284463836769,1.90869858745619));
#24232=CARTESIAN_POINT('Ctrl Pts',(0.946792943618195,0.833432097145889,
1.10727038327973));
#24233=CARTESIAN_POINT('Ctrl Pts',(0.996789604993468,0.903811092885787,
1.18103565901043));
#24234=CARTESIAN_POINT('Ctrl Pts',(1.03588011685503,0.983198189519663,1.25302429310887));
#24235=CARTESIAN_POINT('Ctrl Pts',(1.07809517714267,1.16484813617459,1.39260788389875));
#24236=CARTESIAN_POINT('Ctrl Pts',(1.07820617779495,1.26249969691988,1.45574709063858));
#24237=CARTESIAN_POINT('Ctrl Pts',(1.03816533347023,1.44217179941018,1.55895701082588));
#24238=CARTESIAN_POINT('Ctrl Pts',(1.00786966075201,1.51906903401083,1.5990490209941));
#24239=CARTESIAN_POINT('Ctrl Pts',(0.967951970128401,1.59279130921887,1.63615580822897));
#24240=CARTESIAN_POINT('Ctrl Pts',(0.720016914634041,1.04334803864884,1.1015723109602));
#24241=CARTESIAN_POINT('Ctrl Pts',(0.823064346331371,1.29208090893697,1.31988785480614));
#24242=CARTESIAN_POINT('Ctrl Pts',(0.763481187915705,1.54167481933164,1.49890963328678));
#24243=CARTESIAN_POINT('Ctrl Pts',(0.541267439387044,1.79212976983285,1.63863764640212));
#24244=CARTESIAN_POINT('Ctrl Pts',(0.720837529677195,1.00993315330316,1.12589971949674));
#24245=CARTESIAN_POINT('Ctrl Pts',(0.825567715093924,1.25179094217684,1.34900830339197));
#24246=CARTESIAN_POINT('Ctrl Pts',(0.771065844731941,1.49701757504302,1.53195557707744));
#24247=CARTESIAN_POINT('Ctrl Pts',(0.557477346013133,1.74562013410096,1.67474624941237));
#24248=CARTESIAN_POINT('Ctrl Pts',(0.717530565095653,0.95673563332559,1.16769179538366));
#24249=CARTESIAN_POINT('Ctrl Pts',(0.823961384252209,1.18745042322669,1.39903449435103));
#24250=CARTESIAN_POINT('Ctrl Pts',(0.777060632929278,1.42496257773992,1.58878199846584));
#24251=CARTESIAN_POINT('Ctrl Pts',(0.576871348730713,1.66940588754283,1.73683890344255));
#24252=CARTESIAN_POINT('Ctrl Pts',(0.701101131459801,0.89030854064122,1.22804130170825));
#24253=CARTESIAN_POINT('Ctrl Pts',(0.807060009317124,1.10640797973512,1.47142017171286));
#24254=CARTESIAN_POINT('Ctrl Pts',(0.767978311363819,1.3324357381909,1.67099665961542));
#24255=CARTESIAN_POINT('Ctrl Pts',(0.583845206097281,1.56839818009429,1.82676536339562));
#24256=CARTESIAN_POINT('Ctrl Pts',(0.681352489183287,0.86023395370564,1.2635364344865));
#24257=CARTESIAN_POINT('Ctrl Pts',(0.784556163294565,1.06916866744103,1.51398418220583));
#24258=CARTESIAN_POINT('Ctrl Pts',(0.747275208483436,1.28799335847824,1.71946457116167));
#24259=CARTESIAN_POINT('Ctrl Pts',(0.569616647707433,1.51699586639173,1.87977332297456));
#24260=CARTESIAN_POINT('Ctrl Pts',(0.667616851769879,0.846087143187382,
1.28318517919043));
#24261=CARTESIAN_POINT('Ctrl Pts',(0.768564946360838,1.05147036139454,1.53754499301447));
#24262=CARTESIAN_POINT('Ctrl Pts',(0.731592934569706,1.26643337142018,1.7461278323729));
#24263=CARTESIAN_POINT('Ctrl Pts',(0.55670081639648,1.49097617326428,1.90893369726572));
#24264=CARTESIAN_POINT('',(0.669228599956957,0.849391336665505,1.28727233489076));
#24265=CARTESIAN_POINT('Ctrl Pts',(0.720159740047642,1.03556549162895,1.10727038327973));
#24266=CARTESIAN_POINT('Ctrl Pts',(0.720933639361785,1.00975899746822,1.12801545944058));
#24267=CARTESIAN_POINT('Ctrl Pts',(0.719952669695418,0.981660765603644,
1.15133239961438));
#24268=CARTESIAN_POINT('Ctrl Pts',(0.712287980257497,0.932697144980519,
1.19509600545699));
#24269=CARTESIAN_POINT('Ctrl Pts',(0.70756612481209,0.913389476193535,1.21324740617616));
#24270=CARTESIAN_POINT('Ctrl Pts',(0.694825406569049,0.882563548282451,
1.24538218411057));
#24271=CARTESIAN_POINT('Ctrl Pts',(0.685758102882491,0.866448281269836,
1.26364457694968));
#24272=CARTESIAN_POINT('Ctrl Pts',(0.669228599956957,0.849391336665505,
1.28727233489076));
#24273=CARTESIAN_POINT('Ctrl Pts',(0.669228599956957,0.849391336665505,
1.28727233489076));
#24274=CARTESIAN_POINT('Ctrl Pts',(0.713346345736856,0.940530841324424,
1.39987124007464));
#24275=CARTESIAN_POINT('Ctrl Pts',(0.73033241101646,1.03355488521186,1.50346488650363));
#24276=CARTESIAN_POINT('Ctrl Pts',(0.707591441492497,1.2462884798982,1.715480776583));
#24277=CARTESIAN_POINT('Ctrl Pts',(0.653180259586498,1.36701797678012,1.81902921434248));
#24278=CARTESIAN_POINT('Ctrl Pts',(0.55695325007777,1.49065195897357,1.90869858745619));
#24279=CARTESIAN_POINT('Ctrl Pts',(0.669228599956957,0.849391336665505,
1.28727233489076));
#24280=CARTESIAN_POINT('Ctrl Pts',(0.76842419991163,1.05431200258793,1.54044292999952));
#24281=CARTESIAN_POINT('Ctrl Pts',(0.73045746052879,1.26875982659235,1.74808806061869));
#24282=CARTESIAN_POINT('Ctrl Pts',(0.555328381808437,1.49273480867877,1.91020772674828));
#24283=CARTESIAN_POINT('Ctrl Pts',(0.701662213869994,0.820505999621324,
1.28727233489076));
#24284=CARTESIAN_POINT('Ctrl Pts',(0.808833265245786,1.02095396380933,1.54044292999952));
#24285=CARTESIAN_POINT('Ctrl Pts',(0.779555824624012,1.23640500988538,1.74808806061869));
#24286=CARTESIAN_POINT('Ctrl Pts',(0.613829892004671,1.46685913784949,1.91020772674828));
#24287=CARTESIAN_POINT('Ctrl Pts',(0.734095827783032,0.791620662577144,
1.28727233489076));
#24288=CARTESIAN_POINT('Ctrl Pts',(0.849242330579941,0.98759592503072,1.54044292999952));
#24289=CARTESIAN_POINT('Ctrl Pts',(0.828654188719232,1.20405019317841,1.74808806061869));
#24290=CARTESIAN_POINT('Ctrl Pts',(0.672331402200905,1.44098346702021,1.91020772674828));
#24291=CARTESIAN_POINT('Ctrl Pts',(0.766529441696069,0.762735325532963,
1.28727233489076));
#24292=CARTESIAN_POINT('Ctrl Pts',(0.889651395914097,0.954237886252115,
1.54044292999952));
#24293=CARTESIAN_POINT('Ctrl Pts',(0.877752552814453,1.17169537647143,1.74808806061869));
#24294=CARTESIAN_POINT('Ctrl Pts',(0.730832912397138,1.41510779619092,1.91020772674828));
#24295=CARTESIAN_POINT('Ctrl Pts',(0.669228599956957,0.849391336665505,
1.28727233489076));
#24296=CARTESIAN_POINT('Ctrl Pts',(0.685790285668792,0.835451887202042,
1.28797191329046));
#24297=CARTESIAN_POINT('Ctrl Pts',(0.702160750604669,0.821285101590933,
1.28831907556383));
#24298=CARTESIAN_POINT('Ctrl Pts',(0.718337308749603,0.806883726521852,
1.288319084765));
#24299=CARTESIAN_POINT('Ctrl Pts',(0.73461508960276,0.792392236721716,1.28831909402374));
#24300=CARTESIAN_POINT('Ctrl Pts',(0.7506800644496,0.777677820212488,1.28796761487395));
#24301=CARTESIAN_POINT('Ctrl Pts',(0.766529441696069,0.762735325532963,
1.28727233489076));
#24302=CARTESIAN_POINT('Origin',(0.,0.,1.37171309575435));
#24303=CARTESIAN_POINT('',(1.00491994924733,0.762339710524744,1.10727038327973));
#24304=CARTESIAN_POINT('Ctrl Pts',(1.07301833748062,1.52399042602929,1.63615580822897));
#24305=CARTESIAN_POINT('Ctrl Pts',(1.11607945893996,1.42568690035965,1.5873580551461));
#24306=CARTESIAN_POINT('Ctrl Pts',(1.14151594859478,1.33168344006466,1.53858095020839));
#24307=CARTESIAN_POINT('Ctrl Pts',(1.16157559133822,1.1415374149143,1.42806953503215));
#24308=CARTESIAN_POINT('Ctrl Pts',(1.15142699410503,1.04542790122456,1.36461306044572));
#24309=CARTESIAN_POINT('Ctrl Pts',(1.09387499947176,0.882986840618232,1.23357020765532));
#24310=CARTESIAN_POINT('Ctrl Pts',(1.05413090753298,0.818276751491846,1.17136442658356));
#24311=CARTESIAN_POINT('Ctrl Pts',(1.00491994924733,0.762339710524743,1.10727038327973));
#24312=CARTESIAN_POINT('Origin',(0.,0.,1.10727038327973));
#24313=CARTESIAN_POINT('Ctrl Pts',(0.96185791365589,0.486216001172379,1.28318567027397));
#24314=CARTESIAN_POINT('Ctrl Pts',(1.13989141130718,0.629961036964703,1.53751096017972));
#24315=CARTESIAN_POINT('Ctrl Pts',(1.19690070060403,0.840463183520968,1.74607168007008));
#24316=CARTESIAN_POINT('Ctrl Pts',(1.13288578154644,1.11772244084117,1.90886782994505));
#24317=CARTESIAN_POINT('Ctrl Pts',(0.974277469399888,0.494188516412736,
1.26847940010162));
#24318=CARTESIAN_POINT('Ctrl Pts',(1.15456280023806,0.640136900598344,1.51987665322459));
#24319=CARTESIAN_POINT('Ctrl Pts',(1.2119667709518,0.853518266498017,1.72611612827485));
#24320=CARTESIAN_POINT('Ctrl Pts',(1.14670398409855,1.13450705657511,1.88704325648017));
#24321=CARTESIAN_POINT('Ctrl Pts',(0.999036317271857,0.506068912121109,
1.24117979784214));
#24322=CARTESIAN_POINT('Ctrl Pts',(1.18391556488183,0.655595999565544,1.48716740433065));
#24323=CARTESIAN_POINT('Ctrl Pts',(1.24297220725902,0.874388755352329,1.68888889262423));
#24324=CARTESIAN_POINT('Ctrl Pts',(1.17621563803994,1.16244328394297,1.84634569530463));
#24325=CARTESIAN_POINT('Ctrl Pts',(1.06384465023929,0.515271549474755,1.18072830092663));
#24326=CARTESIAN_POINT('Ctrl Pts',(1.26191264154005,0.669593960494798,1.41461382576643));
#24327=CARTESIAN_POINT('Ctrl Pts',(1.32842099300984,0.89938039390582,1.60644836271615));
#24328=CARTESIAN_POINT('Ctrl Pts',(1.26347706358719,1.20473571427761,1.75614213758938));
#24329=CARTESIAN_POINT('Ctrl Pts',(1.1217813461281,0.508351755467879,1.13430117558029));
#24330=CARTESIAN_POINT('Ctrl Pts',(1.33218043618791,0.663759010940873,1.35902160674437));
#24331=CARTESIAN_POINT('Ctrl Pts',(1.4075118803195,0.901321456978326,1.54332567193682));
#24332=CARTESIAN_POINT('Ctrl Pts',(1.34803978074575,1.22106413381299,1.68715809360678));
#24333=CARTESIAN_POINT('Ctrl Pts',(1.16512794184932,0.498486987186291,1.10192284729582));
#24334=CARTESIAN_POINT('Ctrl Pts',(1.38487268717996,0.653810349677836,1.32027771712106));
#24335=CARTESIAN_POINT('Ctrl Pts',(1.46759648753937,0.896559590305322,1.4993370241196));
#24336=CARTESIAN_POINT('Ctrl Pts',(1.41329934292755,1.22673470906875,1.63910076829144));
#24337=CARTESIAN_POINT('',(0.964710998256926,0.488533777383804,1.28727233489076));
#24338=CARTESIAN_POINT('',(1.15799828028599,0.500065917147829,1.10727038327973));
#24339=CARTESIAN_POINT('Ctrl Pts',(0.964710998256926,0.488533777383804,
1.28727233489076));
#24340=CARTESIAN_POINT('Ctrl Pts',(0.992182562456677,0.506200366158425,
1.25478273943422));
#24341=CARTESIAN_POINT('Ctrl Pts',(1.01873815563839,0.512561466012053,1.22829923781222));
#24342=CARTESIAN_POINT('Ctrl Pts',(1.08065739676596,0.513908711038628,1.172059635034));
#24343=CARTESIAN_POINT('Ctrl Pts',(1.11643729240337,0.510455723374658,1.14130666672621));
#24344=CARTESIAN_POINT('Ctrl Pts',(1.15799828028599,0.500065917147829,1.10727038327973));
#24345=CARTESIAN_POINT('Ctrl Pts',(0.964710998256926,0.488533777383804,
1.28727233489076));
#24346=CARTESIAN_POINT('Ctrl Pts',(1.04310952295002,0.552615413818275,1.39987124007464));
#24347=CARTESIAN_POINT('Ctrl Pts',(1.09769367964031,0.629833086622262,1.50346488650363));
#24348=CARTESIAN_POINT('Ctrl Pts',(1.16666286599128,0.832357123065218,1.715480776583));
#24349=CARTESIAN_POINT('Ctrl Pts',(1.16815913695893,0.964772942765737,1.81902921434248));
#24350=CARTESIAN_POINT('Ctrl Pts',(1.13295228123076,1.11743425489732,1.90869858745619));
#24351=CARTESIAN_POINT('Ctrl Pts',(1.15799828028599,0.500065917147829,1.10727038327973));
#24352=CARTESIAN_POINT('Ctrl Pts',(1.22729623661065,0.55155050162963,1.18103565901047));
#24353=CARTESIAN_POINT('Ctrl Pts',(1.28900548463589,0.61497248470904,1.25302429310896));
#24354=CARTESIAN_POINT('Ctrl Pts',(1.38528731335191,0.774686679112512,1.39260788389887));
#24355=CARTESIAN_POINT('Ctrl Pts',(1.41556887304308,0.867524531197783,1.45574709063869));
#24356=CARTESIAN_POINT('Ctrl Pts',(1.43300950021463,1.05077615643305,1.55895701082594));
#24357=CARTESIAN_POINT('Ctrl Pts',(1.42795915557246,1.13327165021096,1.59904902099413));
#24358=CARTESIAN_POINT('Ctrl Pts',(1.4127766116927,1.21572094522251,1.63615580822897));
#24359=CARTESIAN_POINT('Ctrl Pts',(1.0071890534957,0.769785488061409,1.10157231096021));
#24360=CARTESIAN_POINT('Ctrl Pts',(1.18205566887762,0.97450109754457,1.31988785480615));
#24361=CARTESIAN_POINT('Ctrl Pts',(1.2025174778094,1.23029122098199,1.4989096332868));
#24362=CARTESIAN_POINT('Ctrl Pts',(1.06857448029104,1.53715585837368,1.63863764640214));
#24363=CARTESIAN_POINT('Ctrl Pts',(0.997643737342948,0.737752459617965,
1.12589971949674));
#24364=CARTESIAN_POINT('Ctrl Pts',(1.17198622962025,0.935409478625221,1.34900830339198));
#24365=CARTESIAN_POINT('Ctrl Pts',(1.19593106769121,1.1854758699488,1.53195557707745));
#24366=CARTESIAN_POINT('Ctrl Pts',(1.06961874977298,1.48791342961567,1.67474624941239));
#24367=CARTESIAN_POINT('Ctrl Pts',(0.978058304401187,0.688180702732142,
1.1676928969232));
#24368=CARTESIAN_POINT('Ctrl Pts',(1.15057481942775,0.874714575228634,1.39903559589058));
#24369=CARTESIAN_POINT('Ctrl Pts',(1.17936426310359,1.11509475695032,1.58878350409041));
#24370=CARTESIAN_POINT('Ctrl Pts',(1.06451007676443,1.40943605051226,1.73684040906712));
#24371=CARTESIAN_POINT('Ctrl Pts',(0.941905889318168,0.63008137483939,1.22804259109412));
#24372=CARTESIAN_POINT('Ctrl Pts',(1.10945716971861,0.802861060594562,1.47142146109874));
#24373=CARTESIAN_POINT('Ctrl Pts',(1.14213429484135,1.02990257473199,1.6709984207319));
#24374=CARTESIAN_POINT('Ctrl Pts',(1.0399297097943,1.31121645145953,1.8267671245121));
#24375=CARTESIAN_POINT('Ctrl Pts',(0.913831635565082,0.607581608892784,
1.2635364344865));
#24376=CARTESIAN_POINT('Ctrl Pts',(1.07654853959332,0.77439864068878,1.51398418220584));
#24377=CARTESIAN_POINT('Ctrl Pts',(1.10871279290583,0.994033737629162,1.71946457116168));
#24378=CARTESIAN_POINT('Ctrl Pts',(1.01051512770394,1.26672757950422,1.87977332297458));
#24379=CARTESIAN_POINT('Ctrl Pts',(0.89639666323125,0.598371737953918,1.28318517919043));
#24380=CARTESIAN_POINT('Ctrl Pts',(1.055870911185,0.762508109189138,1.53754499301448));
#24381=CARTESIAN_POINT('Ctrl Pts',(1.08713566171041,0.978375060596136,1.74612783237292));
#24382=CARTESIAN_POINT('Ctrl Pts',(0.990190914807483,1.24597259217491,1.90893369726574));
#24383=CARTESIAN_POINT('',(0.89895057878464,0.601016155111926,1.28727233489076));
#24384=CARTESIAN_POINT('Ctrl Pts',(1.00491994924733,0.762339710524744,1.10727038327973));
#24385=CARTESIAN_POINT('Ctrl Pts',(0.997681325972119,0.737557128050518,
1.12801545944052));
#24386=CARTESIAN_POINT('Ctrl Pts',(0.988065537220638,0.71113725783727,1.15133239961424));
#24387=CARTESIAN_POINT('Ctrl Pts',(0.965645393507445,0.666938606676742,
1.19509600545531));
#24388=CARTESIAN_POINT('Ctrl Pts',(0.955188244340171,0.650035056039365,
1.21324740617484));
#24389=CARTESIAN_POINT('Ctrl Pts',(0.933545365639553,0.624654954884687,
1.24538218411132));
#24390=CARTESIAN_POINT('Ctrl Pts',(0.919941956007271,0.612130376113047,
1.26364457695043));
#24391=CARTESIAN_POINT('Ctrl Pts',(0.89895057878464,0.601016155111926,1.28727233489076));
#24392=CARTESIAN_POINT('Ctrl Pts',(0.89895057878464,0.601016155111926,1.28727233489076));
#24393=CARTESIAN_POINT('Ctrl Pts',(0.969072704191387,0.674061841710201,
1.39987124007464));
#24394=CARTESIAN_POINT('Ctrl Pts',(1.01397342270847,0.757283981982513,1.50346488650363));
#24395=CARTESIAN_POINT('Ctrl Pts',(1.05808377148838,0.966632999495317,1.715480776583));
#24396=CARTESIAN_POINT('Ctrl Pts',(1.04364312863621,1.09826755410688,1.81902921434248));
#24397=CARTESIAN_POINT('Ctrl Pts',(0.990330805779366,1.24558623976355,1.90869858745619));
#24398=CARTESIAN_POINT('Ctrl Pts',(0.89895057878464,0.601016155111926,1.28727233489076));
#24399=CARTESIAN_POINT('Ctrl Pts',(1.056615168778,0.76525416360778,1.54044292999951));
#24400=CARTESIAN_POINT('Ctrl Pts',(1.08677467590956,0.980938531722803,1.74808806061869));
#24401=CARTESIAN_POINT('Ctrl Pts',(0.989429100179332,1.248069259457,1.91020772674828));
#24402=CARTESIAN_POINT('Ctrl Pts',(0.920870718608735,0.563522029202552,
1.28727233489076));
#24403=CARTESIAN_POINT('Ctrl Pts',(1.08473827279984,0.721041695541498,1.54044292999952));
#24404=CARTESIAN_POINT('Ctrl Pts',(1.12347180680941,0.934995043558669,1.74808806061869));
#24405=CARTESIAN_POINT('Ctrl Pts',(1.03707132063747,1.20538207325406,1.91020772674828));
#24406=CARTESIAN_POINT('Ctrl Pts',(0.94279085843283,0.526027903293178,1.28727233489076));
#24407=CARTESIAN_POINT('Ctrl Pts',(1.11286137682168,0.676829227475218,1.54044292999952));
#24408=CARTESIAN_POINT('Ctrl Pts',(1.16016893770927,0.889051555394535,1.74808806061869));
#24409=CARTESIAN_POINT('Ctrl Pts',(1.0847135410956,1.16269488705113,1.91020772674828));
#24410=CARTESIAN_POINT('Ctrl Pts',(0.964710998256926,0.488533777383804,
1.28727233489076));
#24411=CARTESIAN_POINT('Ctrl Pts',(1.14098448084351,0.632616759408936,1.54044292999951));
#24412=CARTESIAN_POINT('Ctrl Pts',(1.19686606860912,0.843108067230401,1.74808806061869));
#24413=CARTESIAN_POINT('Ctrl Pts',(1.13235576155374,1.1200077008482,1.91020772674828));
#24414=CARTESIAN_POINT('Ctrl Pts',(0.89895057878464,0.601016155111926,1.28727233489076));
#24415=CARTESIAN_POINT('Ctrl Pts',(0.910394151125278,0.582641108525671,
1.28797191329047));
#24416=CARTESIAN_POINT('Ctrl Pts',(0.921585610967822,0.564108942884268,
1.28831907556383));
#24417=CARTESIAN_POINT('Ctrl Pts',(0.932520162364073,0.545413589903933,
1.288319084765));
#24418=CARTESIAN_POINT('Ctrl Pts',(0.943523135293241,0.52660125318435,1.28831909402374));
#24419=CARTESIAN_POINT('Ctrl Pts',(0.954254829541784,0.507642661237886,
1.28796761487395));
#24420=CARTESIAN_POINT('Ctrl Pts',(0.964710998256926,0.488533777383804,
1.28727233489076));
#24421=CARTESIAN_POINT('Origin',(0.,0.,1.37171309575435));
#24422=CARTESIAN_POINT('',(1.19131159212569,0.414490807021285,1.10727038327973));
#24423=CARTESIAN_POINT('Ctrl Pts',(1.4914400228729,1.11782012388912,1.63615580822897));
#24424=CARTESIAN_POINT('Ctrl Pts',(1.5020161229969,1.01102129689834,1.58735805514606));
#24425=CARTESIAN_POINT('Ctrl Pts',(1.49715899547356,0.913758385849943,1.53858095020834));
#24426=CARTESIAN_POINT('Ctrl Pts',(1.45747849623498,0.726719999074329,1.42806953503215));
#24427=CARTESIAN_POINT('Ctrl Pts',(1.41812713365386,0.638450508815867,1.36461306044572));
#24428=CARTESIAN_POINT('Ctrl Pts',(1.31319488582046,0.501744424014179,1.23357020765532));
#24429=CARTESIAN_POINT('Ctrl Pts',(1.25539949095026,0.452483071915572,1.17136442658356));
#24430=CARTESIAN_POINT('Ctrl Pts',(1.19131159212569,0.414490807021284,1.10727038327973));
#24431=CARTESIAN_POINT('Origin',(0.,0.,1.10727038327973));
#24432=CARTESIAN_POINT('Ctrl Pts',(1.19577051030242,0.420870970491663,1.1015723109602));
#24433=CARTESIAN_POINT('Ctrl Pts',(1.42533914668799,0.561530328976111,1.31988785480614));
#24434=CARTESIAN_POINT('Ctrl Pts',(1.52384297854318,0.798478145979632,1.49890963328678));
#24435=CARTESIAN_POINT('Ctrl Pts',(1.49128200586798,1.13171442150222,1.63863764640213));
#24436=CARTESIAN_POINT('Ctrl Pts',(1.17679362500493,0.393355414961738,1.12589971949673));
#24437=CARTESIAN_POINT('Ctrl Pts',(1.40368256628313,0.527463617924691,1.34900830339197));
#24438=CARTESIAN_POINT('Ctrl Pts',(1.50373022520314,0.7578915270079,1.53195557707743));
#24439=CARTESIAN_POINT('Ctrl Pts',(1.47705841783302,1.08455939173708,1.67474624941237));
#24440=CARTESIAN_POINT('Ctrl Pts',(1.14284817765567,0.352262141476103,1.16769296545954));
#24441=CARTESIAN_POINT('Ctrl Pts',(1.36456327006819,0.476355861470107,1.39903566442691));
#24442=CARTESIAN_POINT('Ctrl Pts',(1.466225176644,0.696074558068182,1.58878359776798));
#24443=CARTESIAN_POINT('Ctrl Pts',(1.44794881615932,1.01150165877889,1.73684050274469));
#24444=CARTESIAN_POINT('Ctrl Pts',(1.09051150146367,0.30817808510559,1.22804267083047));
#24445=CARTESIAN_POINT('Ctrl Pts',(1.30325409768321,0.420725138053454,1.47142154083508));
#24446=CARTESIAN_POINT('Ctrl Pts',(1.40449154295595,0.626556636662132,1.67099852964048));
#24447=CARTESIAN_POINT('Ctrl Pts',(1.39421997501402,0.925684985930674,1.82676723342069));
#24448=CARTESIAN_POINT('Ctrl Pts',(1.05685857441837,0.295454942931511,1.2635364344865));
#24449=CARTESIAN_POINT('Ctrl Pts',(1.26316084408195,0.403825079433301,1.51398418220583));
#24450=CARTESIAN_POINT('Ctrl Pts',(1.36162184430235,0.602771168700615,1.71946457116167));
#24451=CARTESIAN_POINT('Ctrl Pts',(1.35249734632791,0.892463171324756,1.87977332297457));
#24452=CARTESIAN_POINT('Ctrl Pts',(1.03743092373275,0.292083537908477,1.28318517919043));
#24453=CARTESIAN_POINT('Ctrl Pts',(1.23982087453714,0.398906250549898,1.53754499301447));
#24454=CARTESIAN_POINT('Ctrl Pts',(1.33626197576335,0.594546582101038,1.7461278323729));
#24455=CARTESIAN_POINT('Ctrl Pts',(1.32675422741137,0.879004532561896,1.90893369726572));
#24456=CARTESIAN_POINT('',(1.04067701160391,0.293809324770207,1.28727233489076));
#24457=CARTESIAN_POINT('Ctrl Pts',(1.04067701160391,0.293809324770207,1.28727233489076));
#24458=CARTESIAN_POINT('Ctrl Pts',(1.12993947443311,0.341610972564374,1.39987124007464));
#24459=CARTESIAN_POINT('Ctrl Pts',(1.19835965101752,0.406884846288962,1.50346488650363));
#24460=CARTESIAN_POINT('Ctrl Pts',(1.30500348982786,0.592356746173702,1.715480776583));
#24461=CARTESIAN_POINT('Ctrl Pts',(1.33194693676576,0.722011051157661,1.81902921434248));
#24462=CARTESIAN_POINT('Ctrl Pts',(1.32676788217082,0.878593860895847,1.90869858745619));
#24463=CARTESIAN_POINT('Ctrl Pts',(1.19131159212569,0.414490807021285,1.10727038327973));
#24464=CARTESIAN_POINT('Ctrl Pts',(1.17676901314193,0.393158028076719,1.12801545944028));
#24465=CARTESIAN_POINT('Ctrl Pts',(1.15945966570543,0.371002680489165,1.15133239961405));
#24466=CARTESIAN_POINT('Ctrl Pts',(1.12447870759406,0.335895470715595,1.19509600545462));
#24467=CARTESIAN_POINT('Ctrl Pts',(1.10930988332456,0.323050675538658,1.21324740617407));
#24468=CARTESIAN_POINT('Ctrl Pts',(1.08088339992896,0.305600782276809,1.24538218411082));
#24469=CARTESIAN_POINT('Ctrl Pts',(1.06407548086649,0.297892884779809,1.26364457695002));
#24470=CARTESIAN_POINT('Ctrl Pts',(1.04067701160391,0.293809324770207,1.28727233489076));
#24471=CARTESIAN_POINT('Ctrl Pts',(1.04067701160391,0.293809324770207,1.28727233489076));
#24472=CARTESIAN_POINT('Ctrl Pts',(1.24137728305361,0.401287915254421,1.54044292999952));
#24473=CARTESIAN_POINT('Ctrl Pts',(1.3367108140079,0.59709613876759,1.74808806061869));
#24474=CARTESIAN_POINT('Ctrl Pts',(1.32667760446677,0.881233995309716,1.91020772674828));
#24475=CARTESIAN_POINT('Ctrl Pts',(1.04993798132648,0.251376596276585,1.28727233489076));
#24476=CARTESIAN_POINT('Ctrl Pts',(1.25446154039628,0.35054884232117,1.54044292999952));
#24477=CARTESIAN_POINT('Ctrl Pts',(1.35741454085596,0.542061247874906,1.74808806061869));
#24478=CARTESIAN_POINT('Ctrl Pts',(1.3587969827055,0.825913812937791,1.91020772674828));
#24479=CARTESIAN_POINT('Ctrl Pts',(1.05919895104906,0.208943867782964,1.28727233489076));
#24480=CARTESIAN_POINT('Ctrl Pts',(1.26754579773896,0.29980976938792,1.54044292999952));
#24481=CARTESIAN_POINT('Ctrl Pts',(1.37811826770401,0.487026356982221,1.74808806061869));
#24482=CARTESIAN_POINT('Ctrl Pts',(1.39091636094422,0.770593630565866,1.91020772674828));
#24483=CARTESIAN_POINT('Ctrl Pts',(1.06845992077163,0.166511139289342,1.28727233489076));
#24484=CARTESIAN_POINT('Ctrl Pts',(1.28063005508163,0.24907069645467,1.54044292999952));
#24485=CARTESIAN_POINT('Ctrl Pts',(1.39882199455207,0.431991466089536,1.74808806061869));
#24486=CARTESIAN_POINT('Ctrl Pts',(1.42303573918295,0.715273448193941,1.91020772674828));
#24487=CARTESIAN_POINT('',(1.06845992077163,0.166511139289342,1.28727233489076));
#24488=CARTESIAN_POINT('Ctrl Pts',(1.06845992077163,0.166511139289342,1.28727233489076));
#24489=CARTESIAN_POINT('Ctrl Pts',(1.16282366323453,0.203229920731113,1.39987124007464));
#24490=CARTESIAN_POINT('Ctrl Pts',(1.23859785430383,0.259800859583567,1.50346488650363));
#24491=CARTESIAN_POINT('Ctrl Pts',(1.36677481743678,0.431100013478375,1.715480776583));
#24492=CARTESIAN_POINT('Ctrl Pts',(1.40911659430226,0.556572568507924,1.81902921434248));
#24493=CARTESIAN_POINT('Ctrl Pts',(1.42280782457595,0.712641620935351,1.90869858745619));
#24494=CARTESIAN_POINT('Ctrl Pts',(1.04067701160391,0.293809324770207,1.28727233489076));
#24495=CARTESIAN_POINT('Ctrl Pts',(1.04588229398058,0.272797358647518,1.28797191329046));
#24496=CARTESIAN_POINT('Ctrl Pts',(1.05079925066492,0.251713870469983,1.28831907556383));
#24497=CARTESIAN_POINT('Ctrl Pts',(1.05542144523633,0.230554570986284,1.288319084765));
#24498=CARTESIAN_POINT('Ctrl Pts',(1.06007256258898,0.209262869938632,1.28831909402374));
#24499=CARTESIAN_POINT('Ctrl Pts',(1.06442048323406,0.187915901626936,1.28796761487395));
#24500=CARTESIAN_POINT('Ctrl Pts',(1.06845992077163,0.166511139289342,1.28727233489076));
#24501=CARTESIAN_POINT('Ctrl Pts',(1.06503024383179,0.165188454748262,1.28318567027397));
#24502=CARTESIAN_POINT('Ctrl Pts',(1.27876982080873,0.24688273138137,1.53751096017972));
#24503=CARTESIAN_POINT('Ctrl Pts',(1.39803761752215,0.429465330327861,1.74607168007008));
#24504=CARTESIAN_POINT('Ctrl Pts',(1.42283363397204,0.712936251587734,1.90886782994506));
#24505=CARTESIAN_POINT('Ctrl Pts',(1.07930558594879,0.168932913531384,1.26847940010162));
#24506=CARTESIAN_POINT('Ctrl Pts',(1.29586765564979,0.25202684428835,1.51987665322459));
#24507=CARTESIAN_POINT('Ctrl Pts',(1.41640054440424,0.437225780288049,1.72611612827485));
#24508=CARTESIAN_POINT('Ctrl Pts',(1.44116225705855,0.724629310334688,1.88704325648017));
#24509=CARTESIAN_POINT('Ctrl Pts',(1.10652474870094,0.172580460092753,1.24117906537517));
#24510=CARTESIAN_POINT('Ctrl Pts',(1.32856177300787,0.257658341550684,1.48716667186368));
#24511=CARTESIAN_POINT('Ctrl Pts',(1.45233913898617,0.447493258920483,1.6888878960876));
#24512=CARTESIAN_POINT('Ctrl Pts',(1.47786361346603,0.742078309759803,1.84634469876801));
#24513=CARTESIAN_POINT('Ctrl Pts',(1.171005693206,0.161305070542798,1.18072695962338));
#24514=CARTESIAN_POINT('Ctrl Pts',(1.40706779462019,0.246868029800146,1.41461248446319));
#24515=CARTESIAN_POINT('Ctrl Pts',(1.54132997390971,0.444855864337703,1.60644654213684));
#24516=CARTESIAN_POINT('Ctrl Pts',(1.57392460995617,0.755334809435779,1.75614031701006));
#24517=CARTESIAN_POINT('Ctrl Pts',(1.22396679065338,0.13682174968142,1.13430117558029));
#24518=CARTESIAN_POINT('Ctrl Pts',(1.47209169926766,0.21960593824905,1.35902160674437));
#24519=CARTESIAN_POINT('Ctrl Pts',(1.6171469931418,0.422262554132517,1.54332567193682));
#24520=CARTESIAN_POINT('Ctrl Pts',(1.65939158627328,0.744733799933235,1.68715809360678));
#24521=CARTESIAN_POINT('Ctrl Pts',(1.26214347192869,0.114044962799315,1.10192284729582));
#24522=CARTESIAN_POINT('Ctrl Pts',(1.51913070253036,0.193861398098012,1.32027771712106));
#24523=CARTESIAN_POINT('Ctrl Pts',(1.67281935264038,0.399166585072146,1.4993370241196));
#24524=CARTESIAN_POINT('Ctrl Pts',(1.72320942225876,0.729960523721717,1.63910076829144));
#24525=CARTESIAN_POINT('',(1.25585067703094,0.117749801015222,1.10727038327973));
#24526=CARTESIAN_POINT('Ctrl Pts',(1.25585067703094,0.117749801015222,1.10727038327973));
#24527=CARTESIAN_POINT('Ctrl Pts',(1.33766656151264,0.145300304395604,1.18103565901045));
#24528=CARTESIAN_POINT('Ctrl Pts',(1.4159540145512,0.186548988329726,1.25302429310892));
#24529=CARTESIAN_POINT('Ctrl Pts',(1.55687787546595,0.308693492339194,1.39260788389881));
#24530=CARTESIAN_POINT('Ctrl Pts',(1.61436582414944,0.387630019962978,1.45574709063864));
#24531=CARTESIAN_POINT('Ctrl Pts',(1.68758071271377,0.556523222076105,1.55895701082591));
#24532=CARTESIAN_POINT('Ctrl Pts',(1.70827005906903,0.636541741320481,1.59904902099412));
#24533=CARTESIAN_POINT('Ctrl Pts',(1.71930883511106,0.71964734468187,1.63615580822897));
#24534=CARTESIAN_POINT('Ctrl Pts',(1.06845992077163,0.166511139289342,1.28727233489076));
#24535=CARTESIAN_POINT('Ctrl Pts',(1.10004620708046,0.174823883464324,1.25478273943439));
#24536=CARTESIAN_POINT('Ctrl Pts',(1.12726776497768,0.172667519342153,1.22829923781239));
#24537=CARTESIAN_POINT('Ctrl Pts',(1.18657278434634,0.154814727716086,1.17205963503281));
#24538=CARTESIAN_POINT('Ctrl Pts',(1.21953445537525,0.14047414548817,1.14130666672491));
#24539=CARTESIAN_POINT('Ctrl Pts',(1.25585067703094,0.117749801015222,1.10727038327973));
#24540=CARTESIAN_POINT('Ctrl Pts',(1.2673016181377,0.0307586699497107,1.1015723109602));
#24541=CARTESIAN_POINT('Ctrl Pts',(1.52910049789877,0.0935930593956198,
1.31988785480615));
#24542=CARTESIAN_POINT('Ctrl Pts',(1.69600411129882,0.288504466724436,1.49890963328679));
#24543=CARTESIAN_POINT('Ctrl Pts',(1.76801245833786,0.615492891936159,1.63863764640214));
#24544=CARTESIAN_POINT('Ctrl Pts',(1.23190046521827,0.00368577884439299,
1.13400885567558));
#24545=CARTESIAN_POINT('Ctrl Pts',(1.48760761670895,0.0593992442947171,
1.35870212368824));
#24546=CARTESIAN_POINT('Ctrl Pts',(1.65386565639404,0.245271053169412,1.54297833728479));
#24547=CARTESIAN_POINT('Ctrl Pts',(1.73054693613328,0.56155720138891,1.6867824504158));
#24548=CARTESIAN_POINT('Ctrl Pts',(1.18197455396454,-0.0267745014609978,
1.18052159225508));
#24549=CARTESIAN_POINT('Ctrl Pts',(1.42871036910363,0.0203421811660883,
1.41439816169908));
#24550=CARTESIAN_POINT('Ctrl Pts',(1.59277760615935,0.194600327489428,1.60621915369239));
#24551=CARTESIAN_POINT('Ctrl Pts',(1.67419193839781,0.496164143986696,1.75589578968676));
#24552=CARTESIAN_POINT('Ctrl Pts',(1.11906265670396,-0.0454087437059702,
1.24109759607728));
#24553=CARTESIAN_POINT('Ctrl Pts',(1.35343612743123,-0.00502457427851058,
1.48710236189544));
#24554=CARTESIAN_POINT('Ctrl Pts',(1.51172442238932,0.157227158096703,1.68883153964047));
#24555=CARTESIAN_POINT('Ctrl Pts',(1.59391973364072,0.441350654339689,1.84628730593333));
#24556=CARTESIAN_POINT('Ctrl Pts',(1.09155317863394,-0.0448936420229278,
1.26844862066248));
#24557=CARTESIAN_POINT('Ctrl Pts',(1.32019136139833,-0.00558636246918835,
1.51987386218776));
#24558=CARTESIAN_POINT('Ctrl Pts',(1.47464748824823,0.152483274684963,1.72613059618619));
#24559=CARTESIAN_POINT('Ctrl Pts',(1.55492717401663,0.429627033563921,1.88706341654737));
#24560=CARTESIAN_POINT('Ctrl Pts',(1.07691421721301,-0.0427958338931188,
1.28318517919043));
#24561=CARTESIAN_POINT('Ctrl Pts',(1.30240853234962,-0.00374333123643632,
1.53754499301448));
#24562=CARTESIAN_POINT('Ctrl Pts',(1.45458565734394,0.152519741700297,1.74612783237292));
#24563=CARTESIAN_POINT('Ctrl Pts',(1.53344559219597,0.425993384917079,1.90893369726574));
#24564=CARTESIAN_POINT('',(1.08053472770428,-0.042157609369957,1.28727233489076));
#24565=CARTESIAN_POINT('Ctrl Pts',(1.08053472770428,-0.042157609369957,
1.28727233489076));
#24566=CARTESIAN_POINT('Ctrl Pts',(1.18019989616608,-0.0242791587196548,
1.39987124007464));
#24567=CARTESIAN_POINT('Ctrl Pts',(1.26544208722232,0.0166569869072258,
1.50346488650363));
#24568=CARTESIAN_POINT('Ctrl Pts',(1.42418037408903,0.16009648734447,1.715480776583));
#24569=CARTESIAN_POINT('Ctrl Pts',(1.48987049850469,0.275079075974333,1.81902921434248));
#24570=CARTESIAN_POINT('Ctrl Pts',(1.53333167412,0.425598593400271,1.90869858745619));
#24571=CARTESIAN_POINT('',(1.26108935601086,0.0260686553993157,1.10727038327973));
#24572=CARTESIAN_POINT('Ctrl Pts',(1.26108935601086,0.0260686553993156,
1.10727038327973));
#24573=CARTESIAN_POINT('Ctrl Pts',(1.2406663502733,0.0102738810212643,1.12801545944048));
#24574=CARTESIAN_POINT('Ctrl Pts',(1.21735780368012,-0.00544822415320415,
1.15133239961429));
#24575=CARTESIAN_POINT('Ctrl Pts',(1.17324021107684,-0.0280274542414253,
1.19509600545496));
#24576=CARTESIAN_POINT('Ctrl Pts',(1.15484454191165,-0.0355561559109166,
1.21324740617461));
#24577=CARTESIAN_POINT('Ctrl Pts',(1.12241703607502,-0.0433677241466835,
1.24538218411131));
#24578=CARTESIAN_POINT('Ctrl Pts',(1.10404988380787,-0.0455044376575776,
1.26364457695046));
#24579=CARTESIAN_POINT('Ctrl Pts',(1.08053472770428,-0.0421576093699569,
1.28727233489076));
#24580=CARTESIAN_POINT('Ctrl Pts',(1.76386916735272,0.602229799711917,1.63615580822897));
#24581=CARTESIAN_POINT('Ctrl Pts',(1.74092498377317,0.497389884697104,1.58735805514604));
#24582=CARTESIAN_POINT('Ctrl Pts',(1.70624968855527,0.406388294299235,1.53858095020832));
#24583=CARTESIAN_POINT('Ctrl Pts',(1.61071325107043,0.240766166368977,1.42806953503213));
#24584=CARTESIAN_POINT('Ctrl Pts',(1.54601110868789,0.168977132257998,1.36461306044571));
#24585=CARTESIAN_POINT('Ctrl Pts',(1.40397010717826,0.0713877673286496,
1.23357020765531));
#24586=CARTESIAN_POINT('Ctrl Pts',(1.33378082531076,0.0423971966252646,
1.17136442658356));
#24587=CARTESIAN_POINT('Ctrl Pts',(1.26108935601086,0.0260686553993155,
1.10727038327973));
#24588=CARTESIAN_POINT('Ctrl Pts',(1.08053472770428,-0.042157609369957,
1.28727233489076));
#24589=CARTESIAN_POINT('Ctrl Pts',(1.30462473967982,-0.00195919018135088,
1.54044292999952));
#24590=CARTESIAN_POINT('Ctrl Pts',(1.45580038421926,0.154805815536382,1.74808806061869));
#24591=CARTESIAN_POINT('Ctrl Pts',(1.5340616613226,0.428137407783241,1.91020772674828));
#24592=CARTESIAN_POINT('Ctrl Pts',(1.07622999908393,-0.0853753293366666,
1.28727233489076));
#24593=CARTESIAN_POINT('Ctrl Pts',(1.30138937207125,-0.0542581740029552,
1.54044292999952));
#24594=CARTESIAN_POINT('Ctrl Pts',(1.45848408198029,0.0960667204863551,
1.74808806061869));
#24595=CARTESIAN_POINT('Ctrl Pts',(1.54751412881105,0.365599354131263,1.91020772674828));
#24596=CARTESIAN_POINT('Ctrl Pts',(1.07192527046357,-0.128593049303376,
1.28727233489076));
#24597=CARTESIAN_POINT('Ctrl Pts',(1.29815400446268,-0.106557157824559,
1.54044292999952));
#24598=CARTESIAN_POINT('Ctrl Pts',(1.46116777974132,0.0373276254363271,
1.74808806061869));
#24599=CARTESIAN_POINT('Ctrl Pts',(1.56096659629949,0.303061300479284,1.91020772674828));
#24600=CARTESIAN_POINT('Ctrl Pts',(1.06762054184321,-0.171810769270086,
1.28727233489076));
#24601=CARTESIAN_POINT('Ctrl Pts',(1.29491863685411,-0.158856141646164,
1.54044292999952));
#24602=CARTESIAN_POINT('Ctrl Pts',(1.46385147750235,-0.0214114696136997,
1.74808806061869));
#24603=CARTESIAN_POINT('Ctrl Pts',(1.57441906378793,0.240523246827306,1.91020772674828));
#24604=CARTESIAN_POINT('',(1.06762054184321,-0.171810769270086,1.28727233489076));
#24605=CARTESIAN_POINT('Ctrl Pts',(1.06762054184321,-0.171810769270086,
1.28727233489076));
#24606=CARTESIAN_POINT('Ctrl Pts',(1.16871252149279,-0.166049132983329,
1.39987124007464));
#24607=CARTESIAN_POINT('Ctrl Pts',(1.2582594411694,-0.135662485730195,1.50346488650363));
#24608=CARTESIAN_POINT('Ctrl Pts',(1.43309732687145,-0.0123561690781439,
1.715480776583));
#24609=CARTESIAN_POINT('Ctrl Pts',(1.51213990150266,0.0938909933754471,
1.81902921434248));
#24610=CARTESIAN_POINT('Ctrl Pts',(1.57338902476662,0.238090659850088,1.90869858745619));
#24611=CARTESIAN_POINT('Ctrl Pts',(1.08053472770428,-0.0421576093699569,
1.28727233489076));
#24612=CARTESIAN_POINT('Ctrl Pts',(1.07899219081063,-0.063749697386048,
1.28797191329047));
#24613=CARTESIAN_POINT('Ctrl Pts',(1.07715333835806,-0.085320709379581,
1.28831907556383));
#24614=CARTESIAN_POINT('Ctrl Pts',(1.07501072349525,-0.106872735707655,
1.288319084765));
#24615=CARTESIAN_POINT('Ctrl Pts',(1.07285470149866,-0.128559621036836,
1.28831909402374));
#24616=CARTESIAN_POINT('Ctrl Pts',(1.07039324377381,-0.150205375722348,
1.28796761487395));
#24617=CARTESIAN_POINT('Ctrl Pts',(1.06762054184321,-0.171810769270086,
1.28727233489076));
#24618=CARTESIAN_POINT('Ctrl Pts',(1.06394999323939,-0.172008888562255,
1.28318567027397));
#24619=CARTESIAN_POINT('Ctrl Pts',(1.29246819705105,-0.160362437711244,
1.53750524708654));
#24620=CARTESIAN_POINT('Ctrl Pts',(1.46231724071037,-0.0235777272478809,
1.74606230994598));
#24621=CARTESIAN_POINT('Ctrl Pts',(1.57349712421737,0.238345242827835,1.90885685885231));
#24622=CARTESIAN_POINT('Ctrl Pts',(1.07868660104758,-0.172859184352678,
1.26847655615066));
#24623=CARTESIAN_POINT('Ctrl Pts',(1.3103222134962,-0.160753680728286,1.51986758573726));
#24624=CARTESIAN_POINT('Ctrl Pts',(1.48218330046157,-0.021871343434585,
1.72610301145358));
#24625=CARTESIAN_POINT('Ctrl Pts',(1.59454602809666,0.243802951242388,1.88702818957259));
#24626=CARTESIAN_POINT('Ctrl Pts',(1.10570674896705,-0.177804653077212,
1.24116990569733));
#24627=CARTESIAN_POINT('Ctrl Pts',(1.34316333686973,-0.165504346014847,
1.48715046268483));
#24628=CARTESIAN_POINT('Ctrl Pts',(1.51954463753721,-0.0232151943402924,
1.68886632718445));
#24629=CARTESIAN_POINT('Ctrl Pts',(1.6348527774955,0.24905417978714,1.84632060216323));
#24630=CARTESIAN_POINT('Ctrl Pts',(1.16355922492391,-0.208466679481999,
1.18070487506193));
#24631=CARTESIAN_POINT('Ctrl Pts',(1.41450672434568,-0.200040692821152,
1.41458132511535));
#24632=CARTESIAN_POINT('Ctrl Pts',(1.60338306284494,-0.0532381927575528,
1.60640786607656));
#24633=CARTESIAN_POINT('Ctrl Pts',(1.73033000148215,0.231963750155414,1.75609772232067));
#24634=CARTESIAN_POINT('Ctrl Pts',(1.20636704429046,-0.248125323472877,
1.13427377111504));
#24635=CARTESIAN_POINT('Ctrl Pts',(1.46792997975155,-0.246071577739378,
1.35898374075971));
#24636=CARTESIAN_POINT('Ctrl Pts',(1.66851401508092,-0.0981643196522479,
1.54328012485139));
#24637=CARTESIAN_POINT('Ctrl Pts',(1.80834740097598,0.195461560119271,1.68710766933124));
#24638=CARTESIAN_POINT('Ctrl Pts',(1.23564132105363,-0.2815945488883,1.10188997515679));
#24639=CARTESIAN_POINT('Ctrl Pts',(1.50471693589153,-0.285103641318398,
1.32023346555538));
#24640=CARTESIAN_POINT('Ctrl Pts',(1.71433203676124,-0.137346033394656,
1.49928432698175));
#24641=CARTESIAN_POINT('Ctrl Pts',(1.86448662366276,0.161678274882928,1.63904255943589));
#24642=CARTESIAN_POINT('Ctrl Pts',(1.06762054184321,-0.171810769270086,
1.28727233489076));
#24643=CARTESIAN_POINT('Ctrl Pts',(1.10022966448202,-0.173665579012752,
1.2547827394351));
#24644=CARTESIAN_POINT('Ctrl Pts',(1.12545255134417,-0.184128327165875,
1.22829923781307));
#24645=CARTESIAN_POINT('Ctrl Pts',(1.17633816045211,-0.219433599811049,
1.17205963503587));
#24646=CARTESIAN_POINT('Ctrl Pts',(1.20325508885486,-0.243258020496387,
1.14130666672786));
#24647=CARTESIAN_POINT('Ctrl Pts',(1.23077165948193,-0.27609248605186,1.10727038327973));
#24648=CARTESIAN_POINT('Origin',(0.,0.,1.38794976669063));
#24649=CARTESIAN_POINT('',(-0.7,-8.57252759403147E-17,1.66862915010152));
#24650=CARTESIAN_POINT('Origin',(0.,0.,1.66862915010152));
#24651=CARTESIAN_POINT('',(-0.980679383410898,-1.20098586788396E-16,1.38794976669063));
#24652=CARTESIAN_POINT('Origin',(0.,0.,1.10727038327973));
#24653=CARTESIAN_POINT('Origin',(0.,0.,1.37171309575435));
#24654=CARTESIAN_POINT('Origin',(1.,0.,2.1));
#24655=CARTESIAN_POINT('Origin',(0.541,0.,2.6));
#24656=CARTESIAN_POINT('',(-0.541,-6.62533918338718E-17,2.6));
#24657=CARTESIAN_POINT('Origin',(0.,0.,2.6));
#24658=CARTESIAN_POINT('Origin',(0.,0.,2.58));
#24659=CARTESIAN_POINT('',(-0.501,-6.13548046372824E-17,2.56));
#24660=CARTESIAN_POINT('',(-0.521,-6.38040982355771E-17,2.58));
#24661=CARTESIAN_POINT('Origin',(0.,0.,2.56));
#24662=CARTESIAN_POINT('Origin',(0.,0.,2.13431457505076));
#24663=CARTESIAN_POINT('',(-0.501,-6.13548046372824E-17,1.70862915010152));
#24664=CARTESIAN_POINT('',(-0.501,-6.13548046372824E-17,2.13431457505076));
#24665=CARTESIAN_POINT('Origin',(0.,0.,1.70862915010152));
#24666=CARTESIAN_POINT('Origin',(0.,0.,1.68862915010152));
#24667=CARTESIAN_POINT('',(-0.541,-6.62533918338718E-17,1.66862915010152));
#24668=CARTESIAN_POINT('',(-0.521,-6.38040982355771E-17,1.68862915010152));
#24669=CARTESIAN_POINT('Origin',(0.,0.,1.66862915010152));
#24670=CARTESIAN_POINT('Origin',(0.7,0.,1.66862915010152));
#24671=CARTESIAN_POINT('',(0.,0.,0.));
#24672=CARTESIAN_POINT('Origin',(1.09,0.,3.42));
#24673=CARTESIAN_POINT('',(-1.06,-1.29812560709619E-16,3.42));
#24674=CARTESIAN_POINT('Origin',(0.,0.,3.42));
#24675=CARTESIAN_POINT('',(-0.76,-9.30731567351988E-17,3.42));
#24676=CARTESIAN_POINT('Origin',(0.,0.,3.42));
#24677=CARTESIAN_POINT('Origin',(0.76,0.,3.47));
#24678=CARTESIAN_POINT('',(-1.06,1.29812560709619E-16,3.47));
#24679=CARTESIAN_POINT('Origin',(0.,0.,3.47));
#24680=CARTESIAN_POINT('',(-0.76,-9.30731567351988E-17,3.47));
#24681=CARTESIAN_POINT('Origin',(0.,0.,3.47));
#24682=CARTESIAN_POINT('Origin',(0.,0.,3.445));
#24683=CARTESIAN_POINT('',(-0.76,-9.30731567351988E-17,3.445));
#24684=CARTESIAN_POINT('Origin',(0.,0.,3.1));
#24685=CARTESIAN_POINT('',(-1.06,-1.29812560709619E-16,3.5));
#24686=CARTESIAN_POINT('Origin',(0.,0.,3.5));
#24687=CARTESIAN_POINT('',(-1.06,-1.29812560709619E-16,3.1));
#24688=CARTESIAN_POINT('Origin',(1.09,0.,2.73));
#24689=CARTESIAN_POINT('',(-1.06,-1.29812560709619E-16,2.73));
#24690=CARTESIAN_POINT('Origin',(0.,0.,2.73));
#24691=CARTESIAN_POINT('',(-0.76,-9.30731567351988E-17,2.73));
#24692=CARTESIAN_POINT('Origin',(0.,0.,2.73));
#24693=CARTESIAN_POINT('Origin',(0.76,0.,2.78));
#24694=CARTESIAN_POINT('',(-1.06,1.29812560709619E-16,2.78));
#24695=CARTESIAN_POINT('Origin',(0.,0.,2.78));
#24696=CARTESIAN_POINT('',(-0.76,-9.30731567351988E-17,2.78));
#24697=CARTESIAN_POINT('Origin',(0.,0.,2.78));
#24698=CARTESIAN_POINT('Origin',(0.,0.,2.755));
#24699=CARTESIAN_POINT('',(-0.76,-9.30731567351988E-17,2.755));
#24700=CARTESIAN_POINT('Origin',(0.,0.,3.1));
#24701=CARTESIAN_POINT('',(0.644752300229835,-0.84136464826396,2.9246182449626));
#24702=CARTESIAN_POINT('',(0.676798995897952,-0.815808261267024,2.9246182449626));
#24703=CARTESIAN_POINT('Ctrl Pts',(0.644752300229834,-0.84136464826396,
2.9246182449626));
#24704=CARTESIAN_POINT('Ctrl Pts',(0.650287628305284,-0.837122830502141,
2.92392632269117));
#24705=CARTESIAN_POINT('Ctrl Pts',(0.655704350161558,-0.832884117923057,
2.92360435804703));
#24706=CARTESIAN_POINT('Ctrl Pts',(0.666094029778957,-0.824598624909167,
2.92360435804703));
#24707=CARTESIAN_POINT('Ctrl Pts',(0.671431802990462,-0.820260913860831,
2.92392632269117));
#24708=CARTESIAN_POINT('Ctrl Pts',(0.676798995897952,-0.815808261267023,
2.9246182449626));
#24709=CARTESIAN_POINT('',(1.05980185416667,-0.0204946311236757,2.9246182449626));
#24710=CARTESIAN_POINT('Origin',(0.,0.,2.9246182449626));
#24711=CARTESIAN_POINT('',(1.05980185416667,0.0204946311236757,2.9246182449626));
#24712=CARTESIAN_POINT('Ctrl Pts',(1.05980185416667,-0.0204946311236757,
2.9246182449626));
#24713=CARTESIAN_POINT('Ctrl Pts',(1.05993668810257,-0.013522207252662,
2.92392632269117));
#24714=CARTESIAN_POINT('Ctrl Pts',(1.06,-0.00664444950758591,2.92360435804703));
#24715=CARTESIAN_POINT('Ctrl Pts',(1.06,0.00664444950758591,2.92360435804703));
#24716=CARTESIAN_POINT('Ctrl Pts',(1.05993668810257,0.0135222072526619,
2.92392632269117));
#24717=CARTESIAN_POINT('Ctrl Pts',(1.05980185416667,0.0204946311236757,
2.9246182449626));
#24718=CARTESIAN_POINT('',(0.676798995897952,0.815808261267023,2.9246182449626));
#24719=CARTESIAN_POINT('Origin',(0.,0.,2.9246182449626));
#24720=CARTESIAN_POINT('',(0.644752300229835,0.84136464826396,2.9246182449626));
#24721=CARTESIAN_POINT('Ctrl Pts',(0.676798995897952,0.815808261267023,
2.9246182449626));
#24722=CARTESIAN_POINT('Ctrl Pts',(0.671431802990462,0.820260913860831,
2.92392632269117));
#24723=CARTESIAN_POINT('Ctrl Pts',(0.666094029778957,0.824598624909167,
2.92360435804703));
#24724=CARTESIAN_POINT('Ctrl Pts',(0.655704350161558,0.832884117923057,
2.92360435804703));
#24725=CARTESIAN_POINT('Ctrl Pts',(0.650287628305285,0.83712283050214,2.92392632269117));
#24726=CARTESIAN_POINT('Ctrl Pts',(0.644752300229835,0.84136464826396,2.9246182449626));
#24727=CARTESIAN_POINT('',(-0.215847310465459,1.03779089346786,2.9246182449626));
#24728=CARTESIAN_POINT('Origin',(0.,0.,2.9246182449626));
#24729=CARTESIAN_POINT('',(-0.255808886330142,1.0286699245504,2.9246182449626));
#24730=CARTESIAN_POINT('Ctrl Pts',(-0.215847310465459,1.03779089346786,
2.9246182449626));
#24731=CARTESIAN_POINT('Ctrl Pts',(-0.222674924486219,1.03637083656377,
2.92392632269117));
#24732=CARTESIAN_POINT('Ctrl Pts',(-0.229394330707665,1.03490211602279,
2.92360435804703));
#24733=CARTESIAN_POINT('Ctrl Pts',(-0.242350049279721,1.03194505780268,
2.92360435804703));
#24734=CARTESIAN_POINT('Ctrl Pts',(-0.249041279056074,1.03035288818974,
2.92392632269117));
#24735=CARTESIAN_POINT('Ctrl Pts',(-0.255808886330142,1.0286699245504,2.9246182449626));
#24736=CARTESIAN_POINT('',(-0.945956189565658,0.478295815811116,2.9246182449626));
#24737=CARTESIAN_POINT('Origin',(0.,0.,2.9246182449626));
#24738=CARTESIAN_POINT('',(-0.963740763933195,0.441365766607993,2.9246182449626));
#24739=CARTESIAN_POINT('Ctrl Pts',(-0.945956189565658,0.478295815811116,
2.9246182449626));
#24740=CARTESIAN_POINT('Ctrl Pts',(-0.949102892084109,0.472072381221787,
2.92392632269117));
#24741=CARTESIAN_POINT('Ctrl Pts',(-0.952144081379837,0.465903205615292,
2.92360435804703));
#24742=CARTESIAN_POINT('Ctrl Pts',(-0.957909918573291,0.453930321313932,
2.92360435804703));
#24743=CARTESIAN_POINT('Ctrl Pts',(-0.960837023771914,0.447706205701861,
2.92392632269117));
#24744=CARTESIAN_POINT('Ctrl Pts',(-0.963740763933195,0.441365766607993,
2.9246182449626));
#24745=CARTESIAN_POINT('',(-1.06,-1.29812560709619E-16,2.9246182449626));
#24746=CARTESIAN_POINT('Origin',(0.,0.,2.9246182449626));
#24747=CARTESIAN_POINT('',(-1.06,-1.29812560709619E-16,3.1));
#24748=CARTESIAN_POINT('',(-0.963740763933202,-0.441365766607979,2.9246182449626));
#24749=CARTESIAN_POINT('Origin',(0.,0.,2.9246182449626));
#24750=CARTESIAN_POINT('',(-0.945956189565651,-0.47829581581113,2.9246182449626));
#24751=CARTESIAN_POINT('Ctrl Pts',(-0.963740763933202,-0.441365766607978,
2.9246182449626));
#24752=CARTESIAN_POINT('Ctrl Pts',(-0.960837023771919,-0.447706205701851,
2.92392632269117));
#24753=CARTESIAN_POINT('Ctrl Pts',(-0.957909918573294,-0.453930321313927,
2.92360435804703));
#24754=CARTESIAN_POINT('Ctrl Pts',(-0.952144081379835,-0.465903205615296,
2.92360435804703));
#24755=CARTESIAN_POINT('Ctrl Pts',(-0.949102892084104,-0.472072381221796,
2.92392632269117));
#24756=CARTESIAN_POINT('Ctrl Pts',(-0.945956189565651,-0.47829581581113,
2.9246182449626));
#24757=CARTESIAN_POINT('',(-0.255808886330126,-1.02866992455041,2.9246182449626));
#24758=CARTESIAN_POINT('Origin',(0.,0.,2.9246182449626));
#24759=CARTESIAN_POINT('',(-0.215847310465475,-1.03779089346786,2.9246182449626));
#24760=CARTESIAN_POINT('Ctrl Pts',(-0.255808886330127,-1.02866992455041,
2.9246182449626));
#24761=CARTESIAN_POINT('Ctrl Pts',(-0.249041279056064,-1.03035288818974,
2.92392632269117));
#24762=CARTESIAN_POINT('Ctrl Pts',(-0.242350049279717,-1.03194505780268,
2.92360435804703));
#24763=CARTESIAN_POINT('Ctrl Pts',(-0.22939433070767,-1.03490211602279,
2.92360435804703));
#24764=CARTESIAN_POINT('Ctrl Pts',(-0.222674924486229,-1.03637083656377,
2.92392632269117));
#24765=CARTESIAN_POINT('Ctrl Pts',(-0.215847310465475,-1.03779089346786,
2.9246182449626));
#24766=CARTESIAN_POINT('Origin',(0.,0.,2.9246182449626));
#24767=CARTESIAN_POINT('Origin',(0.56114082167286,-0.703648334221227,3.1));
#24768=CARTESIAN_POINT('',(0.447871167131128,-0.589076750222415,3.2753817550374));
#24769=CARTESIAN_POINT('',(0.461382453375463,-0.578555297026342,3.27639564195297));
#24770=CARTESIAN_POINT('Ctrl Pts',(0.447871167131128,-0.589076750222415,
3.2753817550374));
#24771=CARTESIAN_POINT('Ctrl Pts',(0.452502352671194,-0.585555690407633,
3.27607258736419));
#24772=CARTESIAN_POINT('Ctrl Pts',(0.457039480081211,-0.582018702657134,
3.27639564195297));
#24773=CARTESIAN_POINT('Ctrl Pts',(0.461382453375463,-0.578555297026342,
3.27639564195297));
#24774=CARTESIAN_POINT('',(0.447871167131128,-0.589076750222415,2.9246182449626));
#24775=CARTESIAN_POINT('Ctrl Pts',(0.447871167131128,-0.589076750222415,
2.9246182449626));
#24776=CARTESIAN_POINT('Ctrl Pts',(0.446194419897492,-0.586923529425737,
2.92710779980363));
#24777=CARTESIAN_POINT('Ctrl Pts',(0.444580537728587,-0.584850895382108,
2.92962121790888));
#24778=CARTESIAN_POINT('Ctrl Pts',(0.436672122204369,-0.574693882270445,
2.9424934277131));
#24779=CARTESIAN_POINT('Ctrl Pts',(0.430350710191137,-0.566572846562105,
2.95482825180595));
#24780=CARTESIAN_POINT('Ctrl Pts',(0.419449625073302,-0.552565269832585,
2.98139101419695));
#24781=CARTESIAN_POINT('Ctrl Pts',(0.414869876004012,-0.546678794884774,
2.99561895616294));
#24782=CARTESIAN_POINT('Ctrl Pts',(0.407985330685283,-0.537828888858989,
3.02268687665294));
#24783=CARTESIAN_POINT('Ctrl Pts',(0.40504622519769,-0.534050030841187,
3.03802055188041));
#24784=CARTESIAN_POINT('Ctrl Pts',(0.401219893621933,-0.529130146180412,
3.06935267774138));
#24785=CARTESIAN_POINT('Ctrl Pts',(0.400332631188562,-0.52798915178784,
3.08535112900039));
#24786=CARTESIAN_POINT('Ctrl Pts',(0.400332631188562,-0.52798915178784,
3.11464887099961));
#24787=CARTESIAN_POINT('Ctrl Pts',(0.401219893621933,-0.529130146180413,
3.13064732225863));
#24788=CARTESIAN_POINT('Ctrl Pts',(0.40504622519769,-0.534050030841188,
3.16197944811959));
#24789=CARTESIAN_POINT('Ctrl Pts',(0.407985330685283,-0.537828888858989,
3.17731312334706));
#24790=CARTESIAN_POINT('Ctrl Pts',(0.414869876004012,-0.546678794884774,
3.20438104383706));
#24791=CARTESIAN_POINT('Ctrl Pts',(0.419449625073302,-0.552565269832586,
3.21860898580305));
#24792=CARTESIAN_POINT('Ctrl Pts',(0.430350710191136,-0.566572846562106,
3.24517174819405));
#24793=CARTESIAN_POINT('Ctrl Pts',(0.436672122204372,-0.574693882270443,
3.2575065722869));
#24794=CARTESIAN_POINT('Ctrl Pts',(0.44458053772859,-0.584850895382106,
3.27037878209112));
#24795=CARTESIAN_POINT('Ctrl Pts',(0.446194419897492,-0.586923529425737,
3.27289220019637));
#24796=CARTESIAN_POINT('Ctrl Pts',(0.447871167131128,-0.589076750222415,
3.2753817550374));
#24797=CARTESIAN_POINT('',(0.461382453375463,-0.578555297026342,2.92360435804703));
#24798=CARTESIAN_POINT('Ctrl Pts',(0.461382453375463,-0.578555297026342,
2.92360435804703));
#24799=CARTESIAN_POINT('Ctrl Pts',(0.457039480081211,-0.582018702657134,
2.92360435804703));
#24800=CARTESIAN_POINT('Ctrl Pts',(0.452502352671194,-0.585555690407633,
2.92392741263581));
#24801=CARTESIAN_POINT('Ctrl Pts',(0.447871167131128,-0.589076750222415,
2.9246182449626));
#24802=CARTESIAN_POINT('',(0.56114082167286,-0.703648334221227,2.86185));
#24803=CARTESIAN_POINT('Origin',(0.56114082167286,-0.703648334221227,3.1));
#24804=CARTESIAN_POINT('',(0.474646655807069,-0.56772401052903,2.9246182449626));
#24805=CARTESIAN_POINT('Ctrl Pts',(0.474646655807069,-0.56772401052903,
2.9246182449626));
#24806=CARTESIAN_POINT('Ctrl Pts',(0.470183340581476,-0.571455573060032,
2.92392741263581));
#24807=CARTESIAN_POINT('Ctrl Pts',(0.465725426669714,-0.57509189139555,
2.92360435804703));
#24808=CARTESIAN_POINT('Ctrl Pts',(0.461382453375463,-0.578555297026342,
2.92360435804703));
#24809=CARTESIAN_POINT('',(0.474646655807069,-0.56772401052903,3.2753817550374));
#24810=CARTESIAN_POINT('Ctrl Pts',(0.474646655807069,-0.56772401052903,
3.2753817550374));
#24811=CARTESIAN_POINT('Ctrl Pts',(0.472920532111735,-0.565610166146593,
3.27289220019637));
#24812=CARTESIAN_POINT('Ctrl Pts',(0.47125898589838,-0.56357554291002,3.27037878209112));
#24813=CARTESIAN_POINT('Ctrl Pts',(0.463116418319987,-0.553605259830513,
3.2575065722869));
#24814=CARTESIAN_POINT('Ctrl Pts',(0.456605640437212,-0.545635238363897,
3.24517174819405));
#24815=CARTESIAN_POINT('Ctrl Pts',(0.445374982543132,-0.531890487153133,
3.21860898580305));
#24816=CARTESIAN_POINT('Ctrl Pts',(0.440655183852335,-0.526115698051596,
3.20438104383706));
#24817=CARTESIAN_POINT('Ctrl Pts',(0.433559118901799,-0.517434473303403,
3.17731312334706));
#24818=CARTESIAN_POINT('Ctrl Pts',(0.430529017242169,-0.513728182311292,
3.16197944811959));
#24819=CARTESIAN_POINT('Ctrl Pts',(0.426583923237528,-0.50890300752715,
3.13064732225863));
#24820=CARTESIAN_POINT('Ctrl Pts',(0.425668970421903,-0.507784095477554,
3.11464887099961));
#24821=CARTESIAN_POINT('Ctrl Pts',(0.425668970421903,-0.507784095477554,
3.08535112900039));
#24822=CARTESIAN_POINT('Ctrl Pts',(0.426583923237527,-0.508903007527151,
3.06935267774138));
#24823=CARTESIAN_POINT('Ctrl Pts',(0.430529017242168,-0.513728182311292,
3.03802055188041));
#24824=CARTESIAN_POINT('Ctrl Pts',(0.433559118901799,-0.517434473303403,
3.02268687665294));
#24825=CARTESIAN_POINT('Ctrl Pts',(0.440655183852335,-0.526115698051596,
2.99561895616294));
#24826=CARTESIAN_POINT('Ctrl Pts',(0.445374982543132,-0.531890487153132,
2.98139101419695));
#24827=CARTESIAN_POINT('Ctrl Pts',(0.456605640437212,-0.545635238363897,
2.95482825180595));
#24828=CARTESIAN_POINT('Ctrl Pts',(0.463116418319989,-0.553605259830511,
2.9424934277131));
#24829=CARTESIAN_POINT('Ctrl Pts',(0.471258985898383,-0.563575542910017,
2.92962121790888));
#24830=CARTESIAN_POINT('Ctrl Pts',(0.472920532111735,-0.565610166146593,
2.92710779980363));
#24831=CARTESIAN_POINT('Ctrl Pts',(0.474646655807069,-0.56772401052903,
2.9246182449626));
#24832=CARTESIAN_POINT('Ctrl Pts',(0.461382453375463,-0.578555297026342,
3.27639564195297));
#24833=CARTESIAN_POINT('Ctrl Pts',(0.465725426669714,-0.57509189139555,
3.27639564195297));
#24834=CARTESIAN_POINT('Ctrl Pts',(0.470183340581476,-0.571455573060032,
3.27607258736419));
#24835=CARTESIAN_POINT('Ctrl Pts',(0.474646655807069,-0.56772401052903,
3.2753817550374));
#24836=CARTESIAN_POINT('',(0.56114082167286,-0.703648334221227,3.33815));
#24837=CARTESIAN_POINT('Origin',(0.56114082167286,-0.703648334221227,3.1));
#24838=CARTESIAN_POINT('',(0.644752300229835,-0.84136464826396,3.2753817550374));
#24839=CARTESIAN_POINT('Ctrl Pts',(0.644752300229835,-0.84136464826396,
3.2753817550374));
#24840=CARTESIAN_POINT('Ctrl Pts',(0.646433000359351,-0.843514492555987,
3.27289236009202));
#24841=CARTESIAN_POINT('Ctrl Pts',(0.648050798688572,-0.845583794128261,
3.27037910645452));
#24842=CARTESIAN_POINT('Ctrl Pts',(0.655979290360836,-0.85572466858529,
3.25750707214144));
#24843=CARTESIAN_POINT('Ctrl Pts',(0.662318522702308,-0.863831545066573,
3.24517226455888));
#24844=CARTESIAN_POINT('Ctrl Pts',(0.673252578886601,-0.877812903896684,
3.21860957458692));
#24845=CARTESIAN_POINT('Ctrl Pts',(0.677847358284485,-0.883687417317991,
3.2043816902577));
#24846=CARTESIAN_POINT('Ctrl Pts',(0.684755270452365,-0.892518849463665,
3.17731372034463));
#24847=CARTESIAN_POINT('Ctrl Pts',(0.687704871914685,-0.8962894383426,3.16197991083841));
#24848=CARTESIAN_POINT('Ctrl Pts',(0.691545075614567,-0.901198384221383,
3.13064753590579));
#24849=CARTESIAN_POINT('Ctrl Pts',(0.692435660859823,-0.902336752864262,
3.11464897022091));
#24850=CARTESIAN_POINT('Ctrl Pts',(0.692435660859823,-0.902336752864262,
3.1));
#24851=CARTESIAN_POINT('Ctrl Pts',(0.692435660859823,-0.902336752864262,
3.08535102977909));
#24852=CARTESIAN_POINT('Ctrl Pts',(0.691545075614567,-0.901198384221384,
3.06935246409421));
#24853=CARTESIAN_POINT('Ctrl Pts',(0.687704871914684,-0.896289438342601,
3.03802008916159));
#24854=CARTESIAN_POINT('Ctrl Pts',(0.684755270452365,-0.892518849463665,
3.02268627965537));
#24855=CARTESIAN_POINT('Ctrl Pts',(0.677847358284485,-0.883687417317991,
2.9956183097423));
#24856=CARTESIAN_POINT('Ctrl Pts',(0.6732525788866,-0.877812903896685,2.98139042541308));
#24857=CARTESIAN_POINT('Ctrl Pts',(0.662318522702306,-0.863831545066573,
2.95482773544112));
#24858=CARTESIAN_POINT('Ctrl Pts',(0.655979290360836,-0.85572466858529,
2.94249292785856));
#24859=CARTESIAN_POINT('Ctrl Pts',(0.648050798688553,-0.845583794128238,
2.92962089354545));
#24860=CARTESIAN_POINT('Ctrl Pts',(0.646433000359338,-0.84351449255597,
2.92710763990797));
#24861=CARTESIAN_POINT('Ctrl Pts',(0.644752300229835,-0.84136464826396,
2.9246182449626));
#24862=CARTESIAN_POINT('',(0.676798995897952,-0.815808261267024,3.2753817550374));
#24863=CARTESIAN_POINT('Ctrl Pts',(0.676798995897952,-0.815808261267023,
3.2753817550374));
#24864=CARTESIAN_POINT('Ctrl Pts',(0.671431802990462,-0.820260913860831,
3.27607367730883));
#24865=CARTESIAN_POINT('Ctrl Pts',(0.666094029778957,-0.824598624909167,
3.27639564195297));
#24866=CARTESIAN_POINT('Ctrl Pts',(0.655704350161557,-0.832884117923057,
3.27639564195297));
#24867=CARTESIAN_POINT('Ctrl Pts',(0.650287628305284,-0.837122830502141,
3.27607367730883));
#24868=CARTESIAN_POINT('Ctrl Pts',(0.644752300229834,-0.84136464826396,
3.2753817550374));
#24869=CARTESIAN_POINT('Ctrl Pts',(0.676798995897952,-0.815808261267024,
2.9246182449626));
#24870=CARTESIAN_POINT('Ctrl Pts',(0.678520948142573,-0.817925208095019,
2.92710763990798));
#24871=CARTESIAN_POINT('Ctrl Pts',(0.680178374008934,-0.819962907760957,
2.92962089354548));
#24872=CARTESIAN_POINT('Ctrl Pts',(0.688300740199246,-0.829949172449061,
2.94249292785856));
#24873=CARTESIAN_POINT('Ctrl Pts',(0.694793748460268,-0.837933416726651,
2.95482773544112));
#24874=CARTESIAN_POINT('Ctrl Pts',(0.705991509039913,-0.851704478318938,
2.98139042541308));
#24875=CARTESIAN_POINT('Ctrl Pts',(0.710696301541893,-0.8574912592173,2.9956183097423));
#24876=CARTESIAN_POINT('Ctrl Pts',(0.717769156177965,-0.866191154133894,
3.02268627965537));
#24877=CARTESIAN_POINT('Ctrl Pts',(0.720788860449205,-0.86990583788823,
3.03802008916159));
#24878=CARTESIAN_POINT('Ctrl Pts',(0.72472020309194,-0.874742102885397,
3.06935246409421));
#24879=CARTESIAN_POINT('Ctrl Pts',(0.725631856595695,-0.875863670152773,
3.08535102977909));
#24880=CARTESIAN_POINT('Ctrl Pts',(0.725631856595695,-0.875863670152773,
3.1));
#24881=CARTESIAN_POINT('Ctrl Pts',(0.725631856595695,-0.875863670152773,
3.11464897022091));
#24882=CARTESIAN_POINT('Ctrl Pts',(0.724720203091942,-0.874742102885395,
3.13064753590579));
#24883=CARTESIAN_POINT('Ctrl Pts',(0.720788860449207,-0.869905837888228,
3.16197991083841));
#24884=CARTESIAN_POINT('Ctrl Pts',(0.717769156177965,-0.866191154133894,
3.17731372034463));
#24885=CARTESIAN_POINT('Ctrl Pts',(0.710696301541893,-0.8574912592173,3.2043816902577));
#24886=CARTESIAN_POINT('Ctrl Pts',(0.705991509039915,-0.851704478318937,
3.21860957458692));
#24887=CARTESIAN_POINT('Ctrl Pts',(0.694793748460269,-0.83793341672665,
3.24517226455888));
#24888=CARTESIAN_POINT('Ctrl Pts',(0.688300740199246,-0.829949172449061,
3.25750707214144));
#24889=CARTESIAN_POINT('Ctrl Pts',(0.680178374008915,-0.819962907760934,
3.27037910645455));
#24890=CARTESIAN_POINT('Ctrl Pts',(0.678520948142559,-0.817925208095002,
3.27289236009204));
#24891=CARTESIAN_POINT('Ctrl Pts',(0.676798995897952,-0.815808261267024,
3.2753817550374));
#24892=CARTESIAN_POINT('Origin',(0.,0.,3.1));
#24893=CARTESIAN_POINT('',(-1.06,-1.29812560709619E-16,3.2753817550374));
#24894=CARTESIAN_POINT('',(-1.06,-1.29812560709619E-16,3.1));
#24895=CARTESIAN_POINT('',(-0.963740763933206,0.441365766607969,3.2753817550374));
#24896=CARTESIAN_POINT('Origin',(0.,0.,3.2753817550374));
#24897=CARTESIAN_POINT('',(-0.945956189565646,0.47829581581114,3.2753817550374));
#24898=CARTESIAN_POINT('Ctrl Pts',(-0.963740763933206,0.441365766607969,
3.2753817550374));
#24899=CARTESIAN_POINT('Ctrl Pts',(-0.960837023771922,0.447706205701845,
3.27607367730883));
#24900=CARTESIAN_POINT('Ctrl Pts',(-0.957909918573295,0.453930321313924,
3.27639564195297));
#24901=CARTESIAN_POINT('Ctrl Pts',(-0.952144081379834,0.465903205615299,
3.27639564195297));
#24902=CARTESIAN_POINT('Ctrl Pts',(-0.949102892084101,0.472072381221803,
3.27607367730883));
#24903=CARTESIAN_POINT('Ctrl Pts',(-0.945956189565646,0.47829581581114,
3.2753817550374));
#24904=CARTESIAN_POINT('',(-0.255808886330142,1.0286699245504,3.2753817550374));
#24905=CARTESIAN_POINT('Origin',(0.,0.,3.2753817550374));
#24906=CARTESIAN_POINT('',(-0.215847310465459,1.03779089346786,3.2753817550374));
#24907=CARTESIAN_POINT('Ctrl Pts',(-0.255808886330142,1.0286699245504,3.2753817550374));
#24908=CARTESIAN_POINT('Ctrl Pts',(-0.249041279056074,1.03035288818974,
3.27607367730883));
#24909=CARTESIAN_POINT('Ctrl Pts',(-0.242350049279721,1.03194505780268,
3.27639564195297));
#24910=CARTESIAN_POINT('Ctrl Pts',(-0.229394330707665,1.03490211602279,
3.27639564195297));
#24911=CARTESIAN_POINT('Ctrl Pts',(-0.222674924486219,1.03637083656377,
3.27607367730883));
#24912=CARTESIAN_POINT('Ctrl Pts',(-0.215847310465459,1.03779089346786,
3.2753817550374));
#24913=CARTESIAN_POINT('',(0.644752300229835,0.84136464826396,3.2753817550374));
#24914=CARTESIAN_POINT('Origin',(0.,0.,3.2753817550374));
#24915=CARTESIAN_POINT('',(0.676798995897952,0.815808261267023,3.2753817550374));
#24916=CARTESIAN_POINT('Ctrl Pts',(0.644752300229835,0.84136464826396,3.2753817550374));
#24917=CARTESIAN_POINT('Ctrl Pts',(0.650287628305285,0.83712283050214,3.27607367730883));
#24918=CARTESIAN_POINT('Ctrl Pts',(0.655704350161558,0.832884117923057,
3.27639564195297));
#24919=CARTESIAN_POINT('Ctrl Pts',(0.666094029778957,0.824598624909166,
3.27639564195297));
#24920=CARTESIAN_POINT('Ctrl Pts',(0.671431802990462,0.82026091386083,3.27607367730883));
#24921=CARTESIAN_POINT('Ctrl Pts',(0.676798995897952,0.815808261267023,
3.2753817550374));
#24922=CARTESIAN_POINT('',(1.05980185416667,0.0204946311236757,3.2753817550374));
#24923=CARTESIAN_POINT('Origin',(0.,0.,3.2753817550374));
#24924=CARTESIAN_POINT('',(1.05980185416667,-0.0204946311236757,3.2753817550374));
#24925=CARTESIAN_POINT('Ctrl Pts',(1.05980185416667,0.0204946311236757,
3.2753817550374));
#24926=CARTESIAN_POINT('Ctrl Pts',(1.05993668810257,0.0135222072526619,
3.27607367730883));
#24927=CARTESIAN_POINT('Ctrl Pts',(1.06,0.00664444950758593,3.27639564195297));
#24928=CARTESIAN_POINT('Ctrl Pts',(1.06,-0.0066444495075859,3.27639564195297));
#24929=CARTESIAN_POINT('Ctrl Pts',(1.05993668810257,-0.013522207252662,
3.27607367730883));
#24930=CARTESIAN_POINT('Ctrl Pts',(1.05980185416667,-0.0204946311236757,
3.2753817550374));
#24931=CARTESIAN_POINT('Origin',(0.,0.,3.2753817550374));
#24932=CARTESIAN_POINT('',(-0.215847310465448,-1.03779089346787,3.2753817550374));
#24933=CARTESIAN_POINT('Origin',(0.,0.,3.2753817550374));
#24934=CARTESIAN_POINT('',(-0.255808886330153,-1.0286699245504,3.2753817550374));
#24935=CARTESIAN_POINT('Ctrl Pts',(-0.215847310465448,-1.03779089346787,
3.2753817550374));
#24936=CARTESIAN_POINT('Ctrl Pts',(-0.222674924486212,-1.03637083656377,
3.27607367730883));
#24937=CARTESIAN_POINT('Ctrl Pts',(-0.229394330707662,-1.03490211602279,
3.27639564195297));
#24938=CARTESIAN_POINT('Ctrl Pts',(-0.242350049279725,-1.03194505780268,
3.27639564195297));
#24939=CARTESIAN_POINT('Ctrl Pts',(-0.249041279056081,-1.03035288818974,
3.27607367730883));
#24940=CARTESIAN_POINT('Ctrl Pts',(-0.255808886330153,-1.0286699245504,
3.2753817550374));
#24941=CARTESIAN_POINT('',(-0.945956189565651,-0.47829581581113,3.2753817550374));
#24942=CARTESIAN_POINT('Origin',(0.,0.,3.2753817550374));
#24943=CARTESIAN_POINT('',(-0.963740763933202,-0.441365766607979,3.2753817550374));
#24944=CARTESIAN_POINT('Ctrl Pts',(-0.945956189565651,-0.47829581581113,
3.2753817550374));
#24945=CARTESIAN_POINT('Ctrl Pts',(-0.949102892084104,-0.472072381221796,
3.27607367730883));
#24946=CARTESIAN_POINT('Ctrl Pts',(-0.952144081379835,-0.465903205615296,
3.27639564195297));
#24947=CARTESIAN_POINT('Ctrl Pts',(-0.957909918573294,-0.453930321313927,
3.27639564195297));
#24948=CARTESIAN_POINT('Ctrl Pts',(-0.960837023771919,-0.447706205701851,
3.27607367730883));
#24949=CARTESIAN_POINT('Ctrl Pts',(-0.963740763933202,-0.441365766607978,
3.2753817550374));
#24950=CARTESIAN_POINT('Origin',(0.,0.,3.2753817550374));
#24951=CARTESIAN_POINT('Origin',(0.,0.,3.1));
#24952=CARTESIAN_POINT('Ctrl Pts',(-0.215847310465468,-1.03779089346786,
2.9246182449626));
#24953=CARTESIAN_POINT('Ctrl Pts',(-0.216428786478497,-1.04045706470235,
2.92710763990799));
#24954=CARTESIAN_POINT('Ctrl Pts',(-0.21698853610412,-1.04302337738549,
2.92962089354548));
#24955=CARTESIAN_POINT('Ctrl Pts',(-0.219731899742916,-1.0556000331769,
2.94249292785856));
#24956=CARTESIAN_POINT('Ctrl Pts',(-0.221925908848724,-1.06565456633392,
2.95482773544113));
#24957=CARTESIAN_POINT('Ctrl Pts',(-0.225710868823514,-1.08299544455179,
2.98139042541308));
#24958=CARTESIAN_POINT('Ctrl Pts',(-0.227301766167146,-1.09028179832404,
2.9956183097423));
#24959=CARTESIAN_POINT('Ctrl Pts',(-0.229693765171481,-1.10123587450718,
3.02268627965537));
#24960=CARTESIAN_POINT('Ctrl Pts',(-0.230715267060294,-1.10591284181213,
3.03802008916159));
#24961=CARTESIAN_POINT('Ctrl Pts',(-0.232045259247278,-1.11200185116341,
3.06935246409421));
#24962=CARTESIAN_POINT('Ctrl Pts',(-0.232353729184198,-1.11341389632706,
3.08535102977909));
#24963=CARTESIAN_POINT('Ctrl Pts',(-0.232353729184197,-1.11341389632706,
3.1));
#24964=CARTESIAN_POINT('Ctrl Pts',(-0.232353729184196,-1.11341389632706,
3.11464897022091));
#24965=CARTESIAN_POINT('Ctrl Pts',(-0.232045259247272,-1.11200185116341,
3.13064753590579));
#24966=CARTESIAN_POINT('Ctrl Pts',(-0.230715267060285,-1.10591284181213,
3.16197991083841));
#24967=CARTESIAN_POINT('Ctrl Pts',(-0.229693765171472,-1.10123587450718,
3.17731372034463));
#24968=CARTESIAN_POINT('Ctrl Pts',(-0.227301766167134,-1.09028179832404,
3.2043816902577));
#24969=CARTESIAN_POINT('Ctrl Pts',(-0.225710868823502,-1.08299544455179,
3.21860957458692));
#24970=CARTESIAN_POINT('Ctrl Pts',(-0.221925908848709,-1.06565456633392,
3.24517226455888));
#24971=CARTESIAN_POINT('Ctrl Pts',(-0.219731899742906,-1.05560003317691,
3.25750707214144));
#24972=CARTESIAN_POINT('Ctrl Pts',(-0.216988536104103,-1.04302337738546,
3.27037910645455));
#24973=CARTESIAN_POINT('Ctrl Pts',(-0.216428786478473,-1.04045706470233,
3.27289236009203));
#24974=CARTESIAN_POINT('Ctrl Pts',(-0.215847310465448,-1.03779089346787,
3.2753817550374));
#24975=CARTESIAN_POINT('Origin',(0.,0.,3.1));
#24976=CARTESIAN_POINT('',(-0.147927155402556,-0.725063829393322,2.9246182449626));
#24977=CARTESIAN_POINT('Origin',(0.,0.,2.9246182449626));
#24978=CARTESIAN_POINT('',(-0.164665491127673,-0.72144665501455,2.92360435804703));
#24979=CARTESIAN_POINT('Ctrl Pts',(-0.147927155402556,-0.725063829393322,
2.9246182449626));
#24980=CARTESIAN_POINT('Ctrl Pts',(-0.153627439993726,-0.723900860216853,
2.92392741263581));
#24981=CARTESIAN_POINT('Ctrl Pts',(-0.159249892010255,-0.722682730173013,
2.92360435804703));
#24982=CARTESIAN_POINT('Ctrl Pts',(-0.164665491127673,-0.72144665501455,
2.92360435804703));
#24983=CARTESIAN_POINT('',(-0.181315643661004,-0.717443124828579,2.9246182449626));
#24984=CARTESIAN_POINT('Ctrl Pts',(-0.164665491127673,-0.72144665501455,
2.92360435804703));
#24985=CARTESIAN_POINT('Ctrl Pts',(-0.170081090245091,-0.720210579856086,
2.92360435804703));
#24986=CARTESIAN_POINT('Ctrl Pts',(-0.175675271291411,-0.718868586598702,
2.92392741263581));
#24987=CARTESIAN_POINT('Ctrl Pts',(-0.181315643661004,-0.717443124828579,
2.9246182449626));
#24988=CARTESIAN_POINT('',(-0.659108801429989,-0.336415796117726,2.9246182449626));
#24989=CARTESIAN_POINT('Origin',(0.,0.,2.9246182449626));
#24990=CARTESIAN_POINT('',(-0.66671696224779,-0.321073966946993,2.92360435804703));
#24991=CARTESIAN_POINT('Ctrl Pts',(-0.659108801429989,-0.336415796117726,
2.9246182449626));
#24992=CARTESIAN_POINT('Ctrl Pts',(-0.661753624824974,-0.331234034743915,
2.92392741263581));
#24993=CARTESIAN_POINT('Ctrl Pts',(-0.664306793900707,-0.326078733089052,
2.92360435804703));
#24994=CARTESIAN_POINT('Ctrl Pts',(-0.66671696224779,-0.321073966946993,
2.92360435804703));
#24995=CARTESIAN_POINT('',(-0.673968076611316,-0.305560193266145,2.9246182449626));
#24996=CARTESIAN_POINT('Ctrl Pts',(-0.66671696224779,-0.321073966946993,
2.92360435804703));
#24997=CARTESIAN_POINT('Ctrl Pts',(-0.669127130594873,-0.316069200804934,
2.92360435804703));
#24998=CARTESIAN_POINT('Ctrl Pts',(-0.671565832849124,-0.310858774834149,
2.92392741263581));
#24999=CARTESIAN_POINT('Ctrl Pts',(-0.673968076611316,-0.305560193266145,
2.9246182449626));
#25000=CARTESIAN_POINT('',(-0.74,-9.06238631369041E-17,2.9246182449626));
#25001=CARTESIAN_POINT('Origin',(0.,0.,2.9246182449626));
#25002=CARTESIAN_POINT('',(-0.74,-9.06238631369041E-17,2.7));
#25003=CARTESIAN_POINT('',(-0.74,-9.06238631369041E-17,3.1));
#25004=CARTESIAN_POINT('Origin',(0.,0.,2.7));
#25005=CARTESIAN_POINT('',(-0.673968076611311,0.305560193266154,2.9246182449626));
#25006=CARTESIAN_POINT('Origin',(0.,0.,2.9246182449626));
#25007=CARTESIAN_POINT('',(-0.66671696224779,0.321073966946993,2.92360435804703));
#25008=CARTESIAN_POINT('Ctrl Pts',(-0.673968076611311,0.305560193266154,
2.9246182449626));
#25009=CARTESIAN_POINT('Ctrl Pts',(-0.671565832849121,0.310858774834155,
2.92392741263581));
#25010=CARTESIAN_POINT('Ctrl Pts',(-0.669127130594872,0.316069200804937,
2.92360435804703));
#25011=CARTESIAN_POINT('Ctrl Pts',(-0.66671696224779,0.321073966946993,
2.92360435804703));
#25012=CARTESIAN_POINT('',(-0.659108801429993,0.336415796117718,2.9246182449626));
#25013=CARTESIAN_POINT('Ctrl Pts',(-0.66671696224779,0.321073966946993,
2.92360435804703));
#25014=CARTESIAN_POINT('Ctrl Pts',(-0.664306793900708,0.32607873308905,
2.92360435804703));
#25015=CARTESIAN_POINT('Ctrl Pts',(-0.661753624824977,0.331234034743909,
2.92392741263581));
#25016=CARTESIAN_POINT('Ctrl Pts',(-0.659108801429993,0.336415796117718,
2.9246182449626));
#25017=CARTESIAN_POINT('',(-0.181315643661013,0.717443124828577,2.9246182449626));
#25018=CARTESIAN_POINT('Origin',(0.,0.,2.9246182449626));
#25019=CARTESIAN_POINT('',(-0.164665491127673,0.72144665501455,2.92360435804703));
#25020=CARTESIAN_POINT('Ctrl Pts',(-0.181315643661013,0.717443124828577,
2.9246182449626));
#25021=CARTESIAN_POINT('Ctrl Pts',(-0.175675271291417,0.7188685865987,2.92392741263581));
#25022=CARTESIAN_POINT('Ctrl Pts',(-0.170081090245093,0.720210579856085,
2.92360435804703));
#25023=CARTESIAN_POINT('Ctrl Pts',(-0.164665491127673,0.72144665501455,
2.92360435804703));
#25024=CARTESIAN_POINT('',(-0.147927155402546,0.725063829393324,2.9246182449626));
#25025=CARTESIAN_POINT('Ctrl Pts',(-0.164665491127673,0.72144665501455,
2.92360435804703));
#25026=CARTESIAN_POINT('Ctrl Pts',(-0.159249892010252,0.722682730173014,
2.92360435804703));
#25027=CARTESIAN_POINT('Ctrl Pts',(-0.15362743999372,0.723900860216854,
2.92392741263581));
#25028=CARTESIAN_POINT('Ctrl Pts',(-0.147927155402546,0.725063829393324,
2.9246182449626));
#25029=CARTESIAN_POINT('',(0.447871167131128,0.589076750222415,2.9246182449626));
#25030=CARTESIAN_POINT('Origin',(0.,0.,2.9246182449626));
#25031=CARTESIAN_POINT('',(0.461382453375463,0.578555297026342,2.92360435804703));
#25032=CARTESIAN_POINT('Ctrl Pts',(0.447871167131128,0.589076750222415,
2.9246182449626));
#25033=CARTESIAN_POINT('Ctrl Pts',(0.452502352671194,0.585555690407633,
2.92392741263581));
#25034=CARTESIAN_POINT('Ctrl Pts',(0.457039480081212,0.582018702657134,
2.92360435804703));
#25035=CARTESIAN_POINT('Ctrl Pts',(0.461382453375463,0.578555297026342,
2.92360435804703));
#25036=CARTESIAN_POINT('',(0.474646655807069,0.56772401052903,2.9246182449626));
#25037=CARTESIAN_POINT('Ctrl Pts',(0.461382453375463,0.578555297026342,
2.92360435804703));
#25038=CARTESIAN_POINT('Ctrl Pts',(0.465725426669714,0.57509189139555,2.92360435804703));
#25039=CARTESIAN_POINT('Ctrl Pts',(0.470183340581476,0.571455573060032,
2.92392741263581));
#25040=CARTESIAN_POINT('Ctrl Pts',(0.474646655807069,0.56772401052903,2.9246182449626));
#25041=CARTESIAN_POINT('',(0.739801854166667,0.0171235677229433,2.9246182449626));
#25042=CARTESIAN_POINT('Origin',(0.,0.,2.9246182449626));
#25043=CARTESIAN_POINT('',(0.74,-1.06645361311672E-17,2.92360435804703));
#25044=CARTESIAN_POINT('Ctrl Pts',(0.739801854166667,0.0171235677229433,
2.9246182449626));
#25045=CARTESIAN_POINT('Ctrl Pts',(0.739936475706564,0.0113074161803183,
2.92392741263581));
#25046=CARTESIAN_POINT('Ctrl Pts',(0.74,0.00555487133946257,2.92360435804703));
#25047=CARTESIAN_POINT('Ctrl Pts',(0.74,-1.73472347597681E-18,2.92360435804703));
#25048=CARTESIAN_POINT('',(0.739801854166667,-0.0171235677229433,2.9246182449626));
#25049=CARTESIAN_POINT('Ctrl Pts',(0.74,-1.73472347597681E-18,2.92360435804703));
#25050=CARTESIAN_POINT('Ctrl Pts',(0.74,-0.00555487133946261,2.92360435804703));
#25051=CARTESIAN_POINT('Ctrl Pts',(0.739936475706564,-0.0113074161803182,
2.92392741263581));
#25052=CARTESIAN_POINT('Ctrl Pts',(0.739801854166667,-0.0171235677229433,
2.9246182449626));
#25053=CARTESIAN_POINT('Origin',(0.,0.,2.9246182449626));
#25054=CARTESIAN_POINT('Origin',(0.,0.,3.1));
#25055=CARTESIAN_POINT('',(-0.147927155402543,-0.725063829393324,3.2753817550374));
#25056=CARTESIAN_POINT('Origin',(0.,0.,3.2753817550374));
#25057=CARTESIAN_POINT('Ctrl Pts',(-0.147927155402542,-0.725063829393325,
3.2753817550374));
#25058=CARTESIAN_POINT('Ctrl Pts',(-0.147350705836102,-0.722396331130513,
3.27289220019637));
#25059=CARTESIAN_POINT('Ctrl Pts',(-0.14679593045413,-0.719828715152708,
3.27037878209112));
#25060=CARTESIAN_POINT('Ctrl Pts',(-0.144077657099528,-0.70724622965008,
3.2575065722869));
#25061=CARTESIAN_POINT('Ctrl Pts',(-0.141905847013061,-0.697186671420939,
3.24517174819405));
#25062=CARTESIAN_POINT('Ctrl Pts',(-0.138161968462919,-0.679836477301522,
3.21860898580305));
#25063=CARTESIAN_POINT('Ctrl Pts',(-0.136589802889265,-0.672545867981452,
3.20438104383706));
#25064=CARTESIAN_POINT('Ctrl Pts',(-0.134226872204735,-0.661585285903343,
3.17731312334706));
#25065=CARTESIAN_POINT('Ctrl Pts',(-0.133218414707289,-0.656905422394463,
3.16197944811959));
#25066=CARTESIAN_POINT('Ctrl Pts',(-0.131905667031905,-0.650812576430241,
3.13064732225862));
#25067=CARTESIAN_POINT('Ctrl Pts',(-0.131601330115138,-0.649399607261913,
3.11464887099961));
#25068=CARTESIAN_POINT('Ctrl Pts',(-0.131601330115139,-0.649399607261913,
3.08535112900039));
#25069=CARTESIAN_POINT('Ctrl Pts',(-0.131905667031907,-0.650812576430241,
3.06935267774137));
#25070=CARTESIAN_POINT('Ctrl Pts',(-0.133218414707293,-0.656905422394462,
3.03802055188041));
#25071=CARTESIAN_POINT('Ctrl Pts',(-0.134226872204739,-0.661585285903342,
3.02268687665294));
#25072=CARTESIAN_POINT('Ctrl Pts',(-0.136589802889271,-0.672545867981451,
2.99561895616294));
#25073=CARTESIAN_POINT('Ctrl Pts',(-0.138161968462926,-0.679836477301521,
2.98139101419695));
#25074=CARTESIAN_POINT('Ctrl Pts',(-0.14190584701307,-0.697186671420938,
2.95482825180595));
#25075=CARTESIAN_POINT('Ctrl Pts',(-0.144077657099543,-0.707246229650077,
2.9424934277131));
#25076=CARTESIAN_POINT('Ctrl Pts',(-0.146795930454146,-0.719828715152705,
2.92962121790888));
#25077=CARTESIAN_POINT('Ctrl Pts',(-0.147350705836117,-0.72239633113051,
2.92710779980363));
#25078=CARTESIAN_POINT('Ctrl Pts',(-0.147927155402556,-0.725063829393322,
2.9246182449626));
#25079=CARTESIAN_POINT('Origin',(-0.200268840560683,-0.877435120963641,
3.1));
#25080=CARTESIAN_POINT('',(-0.181315643661016,-0.717443124828576,3.2753817550374));
#25081=CARTESIAN_POINT('',(-0.164665491127673,-0.72144665501455,3.27639564195297));
#25082=CARTESIAN_POINT('Ctrl Pts',(-0.181315643661016,-0.717443124828576,
3.2753817550374));
#25083=CARTESIAN_POINT('Ctrl Pts',(-0.175675271291419,-0.7188685865987,
3.27607258736419));
#25084=CARTESIAN_POINT('Ctrl Pts',(-0.170081090245095,-0.720210579856085,
3.27639564195297));
#25085=CARTESIAN_POINT('Ctrl Pts',(-0.164665491127673,-0.72144665501455,
3.27639564195297));
#25086=CARTESIAN_POINT('Ctrl Pts',(-0.181315643661004,-0.717443124828579,
2.9246182449626));
#25087=CARTESIAN_POINT('Ctrl Pts',(-0.180677622653924,-0.714789679845302,
2.92710779980363));
#25088=CARTESIAN_POINT('Ctrl Pts',(-0.180063411180689,-0.712235629767472,
2.92962121790888));
#25089=CARTESIAN_POINT('Ctrl Pts',(-0.177053154990362,-0.699719787441732,
2.9424934277131));
#25090=CARTESIAN_POINT('Ctrl Pts',(-0.174645209526939,-0.689714125571454,
2.95482825180595));
#25091=CARTESIAN_POINT('Ctrl Pts',(-0.170490360446879,-0.672457732793657,
2.98139101419695));
#25092=CARTESIAN_POINT('Ctrl Pts',(-0.168743555851695,-0.665206983690625,
2.99561895616294));
#25093=CARTESIAN_POINT('Ctrl Pts',(-0.166116864500515,-0.654306603263479,
3.02268687665294));
#25094=CARTESIAN_POINT('Ctrl Pts',(-0.164994936632523,-0.649652638626213,
3.03802055188041));
#25095=CARTESIAN_POINT('Ctrl Pts',(-0.163534094630633,-0.64359359422561,
3.06935267774138));
#25096=CARTESIAN_POINT('Ctrl Pts',(-0.163195228371984,-0.642188506154241,
3.08535112900039));
#25097=CARTESIAN_POINT('Ctrl Pts',(-0.163195228371985,-0.642188506154241,
3.11464887099961));
#25098=CARTESIAN_POINT('Ctrl Pts',(-0.163534094630636,-0.643593594225609,
3.13064732225863));
#25099=CARTESIAN_POINT('Ctrl Pts',(-0.164994936632528,-0.649652638626212,
3.16197944811959));
#25100=CARTESIAN_POINT('Ctrl Pts',(-0.166116864500519,-0.654306603263478,
3.17731312334706));
#25101=CARTESIAN_POINT('Ctrl Pts',(-0.168743555851701,-0.665206983690623,
3.20438104383706));
#25102=CARTESIAN_POINT('Ctrl Pts',(-0.170490360446887,-0.672457732793655,
3.21860898580305));
#25103=CARTESIAN_POINT('Ctrl Pts',(-0.17464520952695,-0.689714125571451,
3.24517174819405));
#25104=CARTESIAN_POINT('Ctrl Pts',(-0.177053154990377,-0.699719787441728,
3.2575065722869));
#25105=CARTESIAN_POINT('Ctrl Pts',(-0.180063411180705,-0.712235629767467,
3.27037878209112));
#25106=CARTESIAN_POINT('Ctrl Pts',(-0.180677622653936,-0.714789679845299,
3.27289220019637));
#25107=CARTESIAN_POINT('Ctrl Pts',(-0.181315643661017,-0.717443124828576,
3.2753817550374));
#25108=CARTESIAN_POINT('',(-0.200268840560683,-0.877435120963641,2.86185));
#25109=CARTESIAN_POINT('Origin',(-0.200268840560683,-0.877435120963641,
3.1));
#25110=CARTESIAN_POINT('Ctrl Pts',(-0.164665491127673,-0.72144665501455,
3.27639564195297));
#25111=CARTESIAN_POINT('Ctrl Pts',(-0.159249892010251,-0.722682730173014,
3.27639564195297));
#25112=CARTESIAN_POINT('Ctrl Pts',(-0.153627439993718,-0.723900860216855,
3.27607258736419));
#25113=CARTESIAN_POINT('Ctrl Pts',(-0.147927155402543,-0.725063829393324,
3.2753817550374));
#25114=CARTESIAN_POINT('',(-0.200268840560683,-0.877435120963641,3.33815));
#25115=CARTESIAN_POINT('Origin',(-0.200268840560683,-0.877435120963641,
3.1));
#25116=CARTESIAN_POINT('Ctrl Pts',(-0.255808886330153,-1.0286699245504,
3.2753817550374));
#25117=CARTESIAN_POINT('Ctrl Pts',(-0.256441802889327,-1.03132435481591,
3.27289236009202));
#25118=CARTESIAN_POINT('Ctrl Pts',(-0.257050967245519,-1.03387938890926,
3.27037910645452));
#25119=CARTESIAN_POINT('Ctrl Pts',(-0.260036088454,-1.04640086511301,3.25750707214144));
#25120=CARTESIAN_POINT('Ctrl Pts',(-0.262421852995025,-1.05641163134326,
3.24517226455888));
#25121=CARTESIAN_POINT('Ctrl Pts',(-0.266535646972229,-1.07367745534592,
3.21860957458692));
#25122=CARTESIAN_POINT('Ctrl Pts',(-0.268263728412826,-1.08093249774324,
3.2043816902577));
#25123=CARTESIAN_POINT('Ctrl Pts',(-0.270861407310783,-1.09183962883285,
3.17731372034463));
#25124=CARTESIAN_POINT('Ctrl Pts',(-0.271970325972461,-1.09649664382985,
3.16197991083841));
#25125=CARTESIAN_POINT('Ctrl Pts',(-0.273413966562287,-1.1025597136748,
3.13064753590579));
#25126=CARTESIAN_POINT('Ctrl Pts',(-0.273748708187842,-1.10396576249696,
3.11464897022091));
#25127=CARTESIAN_POINT('Ctrl Pts',(-0.273748708187841,-1.10396576249696,
3.1));
#25128=CARTESIAN_POINT('Ctrl Pts',(-0.273748708187841,-1.10396576249696,
3.08535102977909));
#25129=CARTESIAN_POINT('Ctrl Pts',(-0.273413966562285,-1.10255971367481,
3.06935246409421));
#25130=CARTESIAN_POINT('Ctrl Pts',(-0.271970325972456,-1.09649664382985,
3.03802008916159));
#25131=CARTESIAN_POINT('Ctrl Pts',(-0.270861407310774,-1.09183962883285,
3.02268627965537));
#25132=CARTESIAN_POINT('Ctrl Pts',(-0.268263728412815,-1.08093249774325,
2.9956183097423));
#25133=CARTESIAN_POINT('Ctrl Pts',(-0.266535646972218,-1.07367745534592,
2.98139042541308));
#25134=CARTESIAN_POINT('Ctrl Pts',(-0.262421852995011,-1.05641163134326,
2.95482773544112));
#25135=CARTESIAN_POINT('Ctrl Pts',(-0.260036088453991,-1.04640086511301,
2.94249292785856));
#25136=CARTESIAN_POINT('Ctrl Pts',(-0.257050967245501,-1.03387938890923,
2.92962089354545));
#25137=CARTESIAN_POINT('Ctrl Pts',(-0.256441802889302,-1.03132435481589,
2.92710763990796));
#25138=CARTESIAN_POINT('Ctrl Pts',(-0.255808886330133,-1.02866992455041,
2.9246182449626));
#25139=CARTESIAN_POINT('Origin',(0.,0.,3.1));
#25140=CARTESIAN_POINT('Ctrl Pts',(-0.945956189565651,-0.47829581581113,
2.9246182449626));
#25141=CARTESIAN_POINT('Ctrl Pts',(-0.94840323053857,-0.479503530132554,
2.92710763990799));
#25142=CARTESIAN_POINT('Ctrl Pts',(-0.950758652771283,-0.480665970039254,
2.92962089354548));
#25143=CARTESIAN_POINT('Ctrl Pts',(-0.962301937464754,-0.486362538606019,
2.94249292785856));
#25144=CARTESIAN_POINT('Ctrl Pts',(-0.971530830331082,-0.490916092100134,
2.95482773544112));
#25145=CARTESIAN_POINT('Ctrl Pts',(-0.98744835880018,-0.498768751956074,
2.98139042541308));
#25146=CARTESIAN_POINT('Ctrl Pts',(-0.994136967841286,-0.502067905597172,
2.9956183097423));
#25147=CARTESIAN_POINT('Ctrl Pts',(-1.00419259644788,-0.50702752025852,
3.02268627965537));
#25148=CARTESIAN_POINT('Ctrl Pts',(-1.00848609273962,-0.509144919340721,
3.03802008916159));
#25149=CARTESIAN_POINT('Ctrl Pts',(-1.01407590851263,-0.511901524811445,
3.06935246409421));
#25150=CARTESIAN_POINT('Ctrl Pts',(-1.01537221773608,-0.512540749062661,
3.08535102977909));
#25151=CARTESIAN_POINT('Ctrl Pts',(-1.01537221773608,-0.512540749062661,
3.1));
#25152=CARTESIAN_POINT('Ctrl Pts',(-1.01537221773608,-0.512540749062661,
3.11464897022091));
#25153=CARTESIAN_POINT('Ctrl Pts',(-1.01407590851263,-0.511901524811445,
3.13064753590579));
#25154=CARTESIAN_POINT('Ctrl Pts',(-1.00848609273962,-0.509144919340721,
3.16197991083841));
#25155=CARTESIAN_POINT('Ctrl Pts',(-1.00419259644788,-0.50702752025852,
3.17731372034463));
#25156=CARTESIAN_POINT('Ctrl Pts',(-0.994136967841286,-0.502067905597172,
3.2043816902577));
#25157=CARTESIAN_POINT('Ctrl Pts',(-0.98744835880018,-0.498768751956074,
3.21860957458692));
#25158=CARTESIAN_POINT('Ctrl Pts',(-0.971530830331082,-0.490916092100134,
3.24517226455888));
#25159=CARTESIAN_POINT('Ctrl Pts',(-0.962301937464754,-0.486362538606019,
3.25750707214144));
#25160=CARTESIAN_POINT('Ctrl Pts',(-0.950758652771256,-0.480665970039241,
3.27037910645455));
#25161=CARTESIAN_POINT('Ctrl Pts',(-0.948403230538551,-0.479503530132544,
3.27289236009204));
#25162=CARTESIAN_POINT('Ctrl Pts',(-0.945956189565651,-0.47829581581113,
3.2753817550374));
#25163=CARTESIAN_POINT('Origin',(0.,0.,3.1));
#25164=CARTESIAN_POINT('',(-0.659108801429989,-0.336415796117726,3.2753817550374));
#25165=CARTESIAN_POINT('Origin',(0.,0.,3.2753817550374));
#25166=CARTESIAN_POINT('Ctrl Pts',(-0.659108801429989,-0.336415796117726,
3.2753817550374));
#25167=CARTESIAN_POINT('Ctrl Pts',(-0.656663856882733,-0.335203324573485,
3.27289220019637));
#25168=CARTESIAN_POINT('Ctrl Pts',(-0.654310517083416,-0.334036183055557,
3.27037878209112));
#25169=CARTESIAN_POINT('Ctrl Pts',(-0.642778318074505,-0.328316363349215,
3.2575065722869));
#25170=CARTESIAN_POINT('Ctrl Pts',(-0.633559337310756,-0.323742320881684,
3.24517174819405));
#25171=CARTESIAN_POINT('Ctrl Pts',(-0.617660139225852,-0.315851733904997,
3.21860898580305));
#25172=CARTESIAN_POINT('Ctrl Pts',(-0.610979882131038,-0.312535281885735,
3.20438104383706));
#25173=CARTESIAN_POINT('Ctrl Pts',(-0.600937290811893,-0.307548884337655,
3.17731312334706));
#25174=CARTESIAN_POINT('Ctrl Pts',(-0.596649663221733,-0.305419480986011,
3.16197944811959));
#25175=CARTESIAN_POINT('Ctrl Pts',(-0.591067599641059,-0.302647001124175,
3.13064732225863));
#25176=CARTESIAN_POINT('Ctrl Pts',(-0.589773144897572,-0.302003969440185,
3.11464887099961));
#25177=CARTESIAN_POINT('Ctrl Pts',(-0.589773144897572,-0.302003969440185,
3.08535112900039));
#25178=CARTESIAN_POINT('Ctrl Pts',(-0.591067599641059,-0.302647001124175,
3.06935267774138));
#25179=CARTESIAN_POINT('Ctrl Pts',(-0.596649663221733,-0.305419480986011,
3.03802055188041));
#25180=CARTESIAN_POINT('Ctrl Pts',(-0.600937290811893,-0.307548884337655,
3.02268687665294));
#25181=CARTESIAN_POINT('Ctrl Pts',(-0.610979882131038,-0.312535281885735,
2.99561895616294));
#25182=CARTESIAN_POINT('Ctrl Pts',(-0.617660139225853,-0.315851733904994,
2.98139101419695));
#25183=CARTESIAN_POINT('Ctrl Pts',(-0.633559337310756,-0.323742320881681,
2.95482825180595));
#25184=CARTESIAN_POINT('Ctrl Pts',(-0.642778318074504,-0.328316363349218,
2.9424934277131));
#25185=CARTESIAN_POINT('Ctrl Pts',(-0.654310517083415,-0.33403618305556,
2.92962121790888));
#25186=CARTESIAN_POINT('Ctrl Pts',(-0.656663856882733,-0.335203324573485,
2.92710779980363));
#25187=CARTESIAN_POINT('Ctrl Pts',(-0.659108801429989,-0.336415796117726,
2.9246182449626));
#25188=CARTESIAN_POINT('Origin',(-0.810871981112177,-0.390495365205802,
3.1));
#25189=CARTESIAN_POINT('',(-0.673968076611316,-0.305560193266145,3.2753817550374));
#25190=CARTESIAN_POINT('',(-0.66671696224779,-0.321073966946993,3.27639564195297));
#25191=CARTESIAN_POINT('Ctrl Pts',(-0.673968076611316,-0.305560193266145,
3.2753817550374));
#25192=CARTESIAN_POINT('Ctrl Pts',(-0.671565832849124,-0.310858774834149,
3.27607258736419));
#25193=CARTESIAN_POINT('Ctrl Pts',(-0.669127130594873,-0.316069200804934,
3.27639564195297));
#25194=CARTESIAN_POINT('Ctrl Pts',(-0.66671696224779,-0.321073966946993,
3.27639564195297));
#25195=CARTESIAN_POINT('Ctrl Pts',(-0.673968076611316,-0.305560193266145,
2.9246182449626));
#25196=CARTESIAN_POINT('Ctrl Pts',(-0.671495730195107,-0.30440462228909,
2.92710779980363));
#25197=CARTESIAN_POINT('Ctrl Pts',(-0.669115938846714,-0.303292407978791,
2.92962121790888));
#25198=CARTESIAN_POINT('Ctrl Pts',(-0.657453795251194,-0.297842420986912,
2.9424934277131));
#25199=CARTESIAN_POINT('Ctrl Pts',(-0.6481297243582,-0.293486600421324,
2.95482825180595));
#25200=CARTESIAN_POINT('Ctrl Pts',(-0.632047627181004,-0.285975807323195,
2.98139101419695));
#25201=CARTESIAN_POINT('Ctrl Pts',(-0.625289648409841,-0.282820746027851,
2.99561895616294));
#25202=CARTESIAN_POINT('Ctrl Pts',(-0.615129672550929,-0.278078099988225,
3.02268687665294));
#25203=CARTESIAN_POINT('Ctrl Pts',(-0.610791545895107,-0.276053559026934,
3.03802055188041));
#25204=CARTESIAN_POINT('Ctrl Pts',(-0.605143574138738,-0.273417938902139,
3.06935267774138));
#25205=CARTESIAN_POINT('Ctrl Pts',(-0.603833752392438,-0.272806817128289,
3.08535112900039));
#25206=CARTESIAN_POINT('Ctrl Pts',(-0.603833752392438,-0.272806817128289,
3.11464887099961));
#25207=CARTESIAN_POINT('Ctrl Pts',(-0.605143574138739,-0.273417938902138,
3.13064732225863));
#25208=CARTESIAN_POINT('Ctrl Pts',(-0.610791545895107,-0.276053559026933,
3.16197944811959));
#25209=CARTESIAN_POINT('Ctrl Pts',(-0.615129672550929,-0.278078099988225,
3.17731312334706));
#25210=CARTESIAN_POINT('Ctrl Pts',(-0.625289648409841,-0.282820746027851,
3.20438104383706));
#25211=CARTESIAN_POINT('Ctrl Pts',(-0.632047627181007,-0.285975807323192,
3.21860898580305));
#25212=CARTESIAN_POINT('Ctrl Pts',(-0.648129724358202,-0.293486600421321,
3.24517174819405));
#25213=CARTESIAN_POINT('Ctrl Pts',(-0.657453795251192,-0.297842420986915,
3.2575065722869));
#25214=CARTESIAN_POINT('Ctrl Pts',(-0.669115938846713,-0.303292407978794,
3.27037878209112));
#25215=CARTESIAN_POINT('Ctrl Pts',(-0.671495730195106,-0.30440462228909,
3.27289220019637));
#25216=CARTESIAN_POINT('Ctrl Pts',(-0.673968076611316,-0.305560193266145,
3.2753817550374));
#25217=CARTESIAN_POINT('',(-0.810871981112177,-0.390495365205802,2.86185));
#25218=CARTESIAN_POINT('Origin',(-0.810871981112177,-0.390495365205802,
3.1));
#25219=CARTESIAN_POINT('Ctrl Pts',(-0.66671696224779,-0.321073966946993,
3.27639564195297));
#25220=CARTESIAN_POINT('Ctrl Pts',(-0.664306793900707,-0.326078733089052,
3.27639564195297));
#25221=CARTESIAN_POINT('Ctrl Pts',(-0.661753624824974,-0.331234034743915,
3.27607258736419));
#25222=CARTESIAN_POINT('Ctrl Pts',(-0.659108801429989,-0.336415796117726,
3.2753817550374));
#25223=CARTESIAN_POINT('',(-0.810871981112177,-0.390495365205802,3.33815));
#25224=CARTESIAN_POINT('Origin',(-0.810871981112177,-0.390495365205802,
3.1));
#25225=CARTESIAN_POINT('Ctrl Pts',(-0.963740763933202,-0.441365766607978,
3.2753817550374));
#25226=CARTESIAN_POINT('Ctrl Pts',(-0.966210698102864,-0.442525942716529,
3.27289236009202));
#25227=CARTESIAN_POINT('Ctrl Pts',(-0.968588111959567,-0.443642716545468,
3.27037910645452));
#25228=CARTESIAN_POINT('Ctrl Pts',(-0.980238988893433,-0.449115867522948,
3.25750707214144));
#25229=CARTESIAN_POINT('Ctrl Pts',(-0.989553220956837,-0.453492212348372,
3.24517226455888));
#25230=CARTESIAN_POINT('Ctrl Pts',(-1.0056170943246,-0.461040983890949,
3.21860957458692));
#25231=CARTESIAN_POINT('Ctrl Pts',(-1.01236675603246,-0.464213360363215,
3.2043816902577));
#25232=CARTESIAN_POINT('Ctrl Pts',(-1.0225139208031,-0.468982898221355,
3.17731372034463));
#25233=CARTESIAN_POINT('Ctrl Pts',(-1.02684632121873,-0.471019512057877,
3.16197991083841));
#25234=CARTESIAN_POINT('Ctrl Pts',(-1.03248671528923,-0.473671090611669,
3.13064753590579));
#25235=CARTESIAN_POINT('Ctrl Pts',(-1.03379471651407,-0.474286036171845,
3.11464897022091));
#25236=CARTESIAN_POINT('Ctrl Pts',(-1.03379471651407,-0.474286036171845,
3.1));
#25237=CARTESIAN_POINT('Ctrl Pts',(-1.03379471651407,-0.474286036171845,
3.08535102977909));
#25238=CARTESIAN_POINT('Ctrl Pts',(-1.03248671528923,-0.473671090611669,
3.06935246409421));
#25239=CARTESIAN_POINT('Ctrl Pts',(-1.02684632121873,-0.471019512057877,
3.03802008916159));
#25240=CARTESIAN_POINT('Ctrl Pts',(-1.0225139208031,-0.468982898221355,
3.02268627965537));
#25241=CARTESIAN_POINT('Ctrl Pts',(-1.01236675603246,-0.464213360363215,
2.9956183097423));
#25242=CARTESIAN_POINT('Ctrl Pts',(-1.0056170943246,-0.461040983890949,
2.98139042541308));
#25243=CARTESIAN_POINT('Ctrl Pts',(-0.989553220956837,-0.453492212348372,
2.95482773544112));
#25244=CARTESIAN_POINT('Ctrl Pts',(-0.980238988893433,-0.449115867522948,
2.94249292785856));
#25245=CARTESIAN_POINT('Ctrl Pts',(-0.96858811195954,-0.443642716545455,
2.92962089354545));
#25246=CARTESIAN_POINT('Ctrl Pts',(-0.966210698102844,-0.44252594271652,
2.92710763990797));
#25247=CARTESIAN_POINT('Ctrl Pts',(-0.963740763933202,-0.441365766607979,
2.9246182449626));
#25248=CARTESIAN_POINT('Origin',(0.,0.,3.1));
#25249=CARTESIAN_POINT('Ctrl Pts',(-0.963740763933198,0.441365766607986,
2.9246182449626));
#25250=CARTESIAN_POINT('Ctrl Pts',(-0.96621069810286,0.442525942716537,
2.92710763990798));
#25251=CARTESIAN_POINT('Ctrl Pts',(-0.968588111959567,0.443642716545468,
2.92962089354548));
#25252=CARTESIAN_POINT('Ctrl Pts',(-0.980238988893433,0.449115867522948,
2.94249292785856));
#25253=CARTESIAN_POINT('Ctrl Pts',(-0.989553220956834,0.453492212348377,
2.95482773544112));
#25254=CARTESIAN_POINT('Ctrl Pts',(-1.0056170943246,0.461040983890953,2.98139042541308));
#25255=CARTESIAN_POINT('Ctrl Pts',(-1.01236675603246,0.464213360363211,
2.9956183097423));
#25256=CARTESIAN_POINT('Ctrl Pts',(-1.02251392080311,0.468982898221349,
3.02268627965537));
#25257=CARTESIAN_POINT('Ctrl Pts',(-1.02684632121873,0.471019512057878,
3.03802008916159));
#25258=CARTESIAN_POINT('Ctrl Pts',(-1.03248671528923,0.473671090611668,
3.06935246409421));
#25259=CARTESIAN_POINT('Ctrl Pts',(-1.03379471651406,0.474286036171856,
3.08535102977909));
#25260=CARTESIAN_POINT('Ctrl Pts',(-1.03379471651406,0.474286036171855,
3.1));
#25261=CARTESIAN_POINT('Ctrl Pts',(-1.03379471651406,0.474286036171854,
3.11464897022091));
#25262=CARTESIAN_POINT('Ctrl Pts',(-1.03248671528923,0.473671090611665,
3.13064753590579));
#25263=CARTESIAN_POINT('Ctrl Pts',(-1.02684632121874,0.471019512057872,
3.16197991083841));
#25264=CARTESIAN_POINT('Ctrl Pts',(-1.02251392080311,0.468982898221341,
3.17731372034463));
#25265=CARTESIAN_POINT('Ctrl Pts',(-1.01236675603247,0.4642133603632,3.2043816902577));
#25266=CARTESIAN_POINT('Ctrl Pts',(-1.00561709432461,0.461040983890937,
3.21860957458692));
#25267=CARTESIAN_POINT('Ctrl Pts',(-0.989553220956842,0.453492212348359,
3.24517226455888));
#25268=CARTESIAN_POINT('Ctrl Pts',(-0.980238988893438,0.449115867522939,
3.25750707214144));
#25269=CARTESIAN_POINT('Ctrl Pts',(-0.968588111959544,0.443642716545446,
3.27037910645455));
#25270=CARTESIAN_POINT('Ctrl Pts',(-0.966210698102848,0.442525942716513,
3.27289236009203));
#25271=CARTESIAN_POINT('Ctrl Pts',(-0.963740763933205,0.441365766607971,
3.2753817550374));
#25272=CARTESIAN_POINT('Origin',(0.,0.,3.1));
#25273=CARTESIAN_POINT('',(-0.74,-9.06238631369041E-17,3.2753817550374));
#25274=CARTESIAN_POINT('Origin',(0.,0.,3.2753817550374));
#25275=CARTESIAN_POINT('',(-0.673968076611317,0.305560193266142,3.2753817550374));
#25276=CARTESIAN_POINT('Origin',(0.,0.,3.2753817550374));
#25277=CARTESIAN_POINT('Ctrl Pts',(-0.673968076611317,0.305560193266142,
3.2753817550374));
#25278=CARTESIAN_POINT('Ctrl Pts',(-0.671495730195108,0.304404622289088,
3.27289220019637));
#25279=CARTESIAN_POINT('Ctrl Pts',(-0.669115938846715,0.303292407978788,
3.27037878209112));
#25280=CARTESIAN_POINT('Ctrl Pts',(-0.657453795251195,0.29784242098691,
3.2575065722869));
#25281=CARTESIAN_POINT('Ctrl Pts',(-0.648129724358203,0.293486600421318,
3.24517174819405));
#25282=CARTESIAN_POINT('Ctrl Pts',(-0.632047627181007,0.28597580732319,
3.21860898580305));
#25283=CARTESIAN_POINT('Ctrl Pts',(-0.625289648409841,0.282820746027851,
3.20438104383706));
#25284=CARTESIAN_POINT('Ctrl Pts',(-0.615129672550928,0.278078099988226,
3.17731312334706));
#25285=CARTESIAN_POINT('Ctrl Pts',(-0.610791545895108,0.276053559026932,
3.16197944811959));
#25286=CARTESIAN_POINT('Ctrl Pts',(-0.605143574138739,0.273417938902138,
3.13064732225863));
#25287=CARTESIAN_POINT('Ctrl Pts',(-0.603833752392439,0.272806817128288,
3.11464887099961));
#25288=CARTESIAN_POINT('Ctrl Pts',(-0.603833752392438,0.272806817128289,
3.08535112900039));
#25289=CARTESIAN_POINT('Ctrl Pts',(-0.605143574138737,0.273417938902141,
3.06935267774137));
#25290=CARTESIAN_POINT('Ctrl Pts',(-0.610791545895105,0.276053559026937,
3.03802055188041));
#25291=CARTESIAN_POINT('Ctrl Pts',(-0.615129672550927,0.278078099988229,
3.02268687665294));
#25292=CARTESIAN_POINT('Ctrl Pts',(-0.625289648409839,0.282820746027856,
2.99561895616294));
#25293=CARTESIAN_POINT('Ctrl Pts',(-0.632047627181002,0.285975807323201,
2.98139101419695));
#25294=CARTESIAN_POINT('Ctrl Pts',(-0.648129724358197,0.293486600421331,
2.95482825180595));
#25295=CARTESIAN_POINT('Ctrl Pts',(-0.65745379525119,0.297842420986921,
2.9424934277131));
#25296=CARTESIAN_POINT('Ctrl Pts',(-0.66911593884671,0.3032924079788,2.92962121790888));
#25297=CARTESIAN_POINT('Ctrl Pts',(-0.671495730195102,0.304404622289099,
2.92710779980363));
#25298=CARTESIAN_POINT('Ctrl Pts',(-0.673968076611311,0.305560193266154,
2.9246182449626));
#25299=CARTESIAN_POINT('Origin',(-0.810871981112177,0.390495365205802,3.1));
#25300=CARTESIAN_POINT('',(-0.659108801429987,0.336415796117729,3.2753817550374));
#25301=CARTESIAN_POINT('',(-0.66671696224779,0.321073966946993,3.27639564195297));
#25302=CARTESIAN_POINT('Ctrl Pts',(-0.659108801429987,0.336415796117729,
3.2753817550374));
#25303=CARTESIAN_POINT('Ctrl Pts',(-0.661753624824973,0.331234034743917,
3.27607258736419));
#25304=CARTESIAN_POINT('Ctrl Pts',(-0.664306793900707,0.326078733089053,
3.27639564195297));
#25305=CARTESIAN_POINT('Ctrl Pts',(-0.66671696224779,0.321073966946993,
3.27639564195297));
#25306=CARTESIAN_POINT('Ctrl Pts',(-0.659108801429993,0.336415796117718,
2.9246182449626));
#25307=CARTESIAN_POINT('Ctrl Pts',(-0.656663856882737,0.335203324573476,
2.92710779980363));
#25308=CARTESIAN_POINT('Ctrl Pts',(-0.654310517083419,0.334036183055551,
2.92962121790888));
#25309=CARTESIAN_POINT('Ctrl Pts',(-0.642778318074508,0.32831636334921,
2.9424934277131));
#25310=CARTESIAN_POINT('Ctrl Pts',(-0.633559337310759,0.323742320881676,
2.95482825180595));
#25311=CARTESIAN_POINT('Ctrl Pts',(-0.617660139225855,0.31585173390499,
2.98139101419695));
#25312=CARTESIAN_POINT('Ctrl Pts',(-0.61097988213104,0.31253528188573,2.99561895616294));
#25313=CARTESIAN_POINT('Ctrl Pts',(-0.600937290811895,0.307548884337651,
3.02268687665294));
#25314=CARTESIAN_POINT('Ctrl Pts',(-0.596649663221735,0.305419480986006,
3.03802055188041));
#25315=CARTESIAN_POINT('Ctrl Pts',(-0.591067599641061,0.302647001124171,
3.06935267774138));
#25316=CARTESIAN_POINT('Ctrl Pts',(-0.589773144897572,0.302003969440184,
3.08535112900039));
#25317=CARTESIAN_POINT('Ctrl Pts',(-0.589773144897571,0.302003969440185,
3.11464887099961));
#25318=CARTESIAN_POINT('Ctrl Pts',(-0.591067599641059,0.302647001124175,
3.13064732225862));
#25319=CARTESIAN_POINT('Ctrl Pts',(-0.596649663221732,0.305419480986012,
3.16197944811959));
#25320=CARTESIAN_POINT('Ctrl Pts',(-0.600937290811894,0.307548884337654,
3.17731312334706));
#25321=CARTESIAN_POINT('Ctrl Pts',(-0.610979882131038,0.312535281885736,
3.20438104383706));
#25322=CARTESIAN_POINT('Ctrl Pts',(-0.61766013922585,0.315851733905002,
3.21860898580305));
#25323=CARTESIAN_POINT('Ctrl Pts',(-0.633559337310753,0.32374232088169,
3.24517174819405));
#25324=CARTESIAN_POINT('Ctrl Pts',(-0.642778318074502,0.32831636334922,
3.2575065722869));
#25325=CARTESIAN_POINT('Ctrl Pts',(-0.654310517083413,0.334036183055563,
3.27037878209112));
#25326=CARTESIAN_POINT('Ctrl Pts',(-0.656663856882731,0.335203324573488,
3.27289220019637));
#25327=CARTESIAN_POINT('Ctrl Pts',(-0.659108801429987,0.336415796117729,
3.2753817550374));
#25328=CARTESIAN_POINT('',(-0.810871981112177,0.390495365205802,2.86185));
#25329=CARTESIAN_POINT('Origin',(-0.810871981112177,0.390495365205802,3.1));
#25330=CARTESIAN_POINT('Ctrl Pts',(-0.66671696224779,0.321073966946993,
3.27639564195297));
#25331=CARTESIAN_POINT('Ctrl Pts',(-0.669127130594873,0.316069200804933,
3.27639564195297));
#25332=CARTESIAN_POINT('Ctrl Pts',(-0.671565832849125,0.310858774834148,
3.27607258736419));
#25333=CARTESIAN_POINT('Ctrl Pts',(-0.673968076611317,0.305560193266142,
3.2753817550374));
#25334=CARTESIAN_POINT('',(-0.810871981112177,0.390495365205802,3.33815));
#25335=CARTESIAN_POINT('Origin',(-0.810871981112177,0.390495365205802,3.1));
#25336=CARTESIAN_POINT('Ctrl Pts',(-0.945956189565646,0.47829581581114,
3.2753817550374));
#25337=CARTESIAN_POINT('Ctrl Pts',(-0.948403230538565,0.479503530132563,
3.27289236009202));
#25338=CARTESIAN_POINT('Ctrl Pts',(-0.950758652771278,0.480665970039264,
3.27037910645452));
#25339=CARTESIAN_POINT('Ctrl Pts',(-0.962301937464749,0.486362538606029,
3.25750707214144));
#25340=CARTESIAN_POINT('Ctrl Pts',(-0.971530830331079,0.490916092100141,
3.24517226455888));
#25341=CARTESIAN_POINT('Ctrl Pts',(-0.987448358800177,0.49876875195608,
3.21860957458692));
#25342=CARTESIAN_POINT('Ctrl Pts',(-0.994136967841278,0.502067905597186,
3.2043816902577));
#25343=CARTESIAN_POINT('Ctrl Pts',(-1.00419259644787,0.507027520258534,
3.17731372034463));
#25344=CARTESIAN_POINT('Ctrl Pts',(-1.00848609273961,0.509144919340726,
3.16197991083841));
#25345=CARTESIAN_POINT('Ctrl Pts',(-1.01407590851262,0.511901524811448,
3.13064753590579));
#25346=CARTESIAN_POINT('Ctrl Pts',(-1.01537221773608,0.512540749062652,
3.11464897022091));
#25347=CARTESIAN_POINT('Ctrl Pts',(-1.01537221773608,0.512540749062652,
3.1));
#25348=CARTESIAN_POINT('Ctrl Pts',(-1.01537221773609,0.512540749062651,
3.08535102977909));
#25349=CARTESIAN_POINT('Ctrl Pts',(-1.01407590851262,0.511901524811446,
3.06935246409421));
#25350=CARTESIAN_POINT('Ctrl Pts',(-1.00848609273962,0.509144919340721,
3.03802008916159));
#25351=CARTESIAN_POINT('Ctrl Pts',(-1.00419259644788,0.507027520258526,
3.02268627965537));
#25352=CARTESIAN_POINT('Ctrl Pts',(-0.994136967841284,0.502067905597176,
2.9956183097423));
#25353=CARTESIAN_POINT('Ctrl Pts',(-0.987448358800183,0.498768751956068,
2.98139042541308));
#25354=CARTESIAN_POINT('Ctrl Pts',(-0.971530830331086,0.490916092100127,
2.95482773544112));
#25355=CARTESIAN_POINT('Ctrl Pts',(-0.962301937464754,0.48636253860602,
2.94249292785856));
#25356=CARTESIAN_POINT('Ctrl Pts',(-0.950758652771256,0.480665970039241,
2.92962089354545));
#25357=CARTESIAN_POINT('Ctrl Pts',(-0.948403230538554,0.479503530132536,
2.92710763990796));
#25358=CARTESIAN_POINT('Ctrl Pts',(-0.945956189565655,0.478295815811122,
2.9246182449626));
#25359=CARTESIAN_POINT('Origin',(0.,0.,3.1));
#25360=CARTESIAN_POINT('Ctrl Pts',(-0.255808886330142,1.0286699245504,2.9246182449626));
#25361=CARTESIAN_POINT('Ctrl Pts',(-0.256441802889316,1.03132435481591,
2.92710763990798));
#25362=CARTESIAN_POINT('Ctrl Pts',(-0.257050967245508,1.03387938890926,
2.92962089354548));
#25363=CARTESIAN_POINT('Ctrl Pts',(-0.26003608845399,1.04640086511301,2.94249292785856));
#25364=CARTESIAN_POINT('Ctrl Pts',(-0.262421852995016,1.05641163134326,
2.95482773544112));
#25365=CARTESIAN_POINT('Ctrl Pts',(-0.266535646972222,1.07367745534592,
2.98139042541308));
#25366=CARTESIAN_POINT('Ctrl Pts',(-0.26826372841281,1.08093249774325,2.9956183097423));
#25367=CARTESIAN_POINT('Ctrl Pts',(-0.270861407310768,1.09183962883285,
3.02268627965537));
#25368=CARTESIAN_POINT('Ctrl Pts',(-0.271970325972459,1.09649664382985,
3.03802008916159));
#25369=CARTESIAN_POINT('Ctrl Pts',(-0.273413966562286,1.1025597136748,3.06935246409421));
#25370=CARTESIAN_POINT('Ctrl Pts',(-0.273748708187841,1.10396576249696,
3.08535102977909));
#25371=CARTESIAN_POINT('Ctrl Pts',(-0.273748708187841,1.10396576249696,
3.1));
#25372=CARTESIAN_POINT('Ctrl Pts',(-0.273748708187841,1.10396576249696,
3.11464897022091));
#25373=CARTESIAN_POINT('Ctrl Pts',(-0.273413966562286,1.1025597136748,3.13064753590579));
#25374=CARTESIAN_POINT('Ctrl Pts',(-0.271970325972459,1.09649664382985,
3.16197991083841));
#25375=CARTESIAN_POINT('Ctrl Pts',(-0.270861407310768,1.09183962883285,
3.17731372034463));
#25376=CARTESIAN_POINT('Ctrl Pts',(-0.26826372841281,1.08093249774325,3.2043816902577));
#25377=CARTESIAN_POINT('Ctrl Pts',(-0.266535646972222,1.07367745534592,
3.21860957458692));
#25378=CARTESIAN_POINT('Ctrl Pts',(-0.262421852995016,1.05641163134326,
3.24517226455888));
#25379=CARTESIAN_POINT('Ctrl Pts',(-0.26003608845399,1.04640086511301,3.25750707214144));
#25380=CARTESIAN_POINT('Ctrl Pts',(-0.257050967245501,1.03387938890923,
3.27037910645455));
#25381=CARTESIAN_POINT('Ctrl Pts',(-0.256441802889309,1.03132435481589,
3.27289236009204));
#25382=CARTESIAN_POINT('Ctrl Pts',(-0.25580888633014,1.0286699245504,3.2753817550374));
#25383=CARTESIAN_POINT('Origin',(0.,0.,3.1));
#25384=CARTESIAN_POINT('',(-0.181315643661013,0.717443124828577,3.2753817550374));
#25385=CARTESIAN_POINT('Origin',(0.,0.,3.2753817550374));
#25386=CARTESIAN_POINT('Ctrl Pts',(-0.181315643661013,0.717443124828577,
3.2753817550374));
#25387=CARTESIAN_POINT('Ctrl Pts',(-0.180677622653932,0.7147896798453,3.27289220019637));
#25388=CARTESIAN_POINT('Ctrl Pts',(-0.180063411180699,0.712235629767469,
3.27037878209112));
#25389=CARTESIAN_POINT('Ctrl Pts',(-0.177053154990371,0.699719787441729,
3.2575065722869));
#25390=CARTESIAN_POINT('Ctrl Pts',(-0.174645209526945,0.689714125571452,
3.24517174819405));
#25391=CARTESIAN_POINT('Ctrl Pts',(-0.170490360446883,0.672457732793656,
3.21860898580305));
#25392=CARTESIAN_POINT('Ctrl Pts',(-0.1687435558517,0.665206983690623,3.20438104383706));
#25393=CARTESIAN_POINT('Ctrl Pts',(-0.166116864500519,0.654306603263478,
3.17731312334706));
#25394=CARTESIAN_POINT('Ctrl Pts',(-0.164994936632528,0.649652638626212,
3.16197944811959));
#25395=CARTESIAN_POINT('Ctrl Pts',(-0.163534094630637,0.643593594225609,
3.13064732225863));
#25396=CARTESIAN_POINT('Ctrl Pts',(-0.163195228371982,0.642188506154242,
3.11464887099961));
#25397=CARTESIAN_POINT('Ctrl Pts',(-0.163195228371982,0.642188506154242,
3.08535112900039));
#25398=CARTESIAN_POINT('Ctrl Pts',(-0.163534094630636,0.643593594225609,
3.06935267774138));
#25399=CARTESIAN_POINT('Ctrl Pts',(-0.164994936632526,0.649652638626212,
3.03802055188041));
#25400=CARTESIAN_POINT('Ctrl Pts',(-0.166116864500519,0.654306603263478,
3.02268687665294));
#25401=CARTESIAN_POINT('Ctrl Pts',(-0.1687435558517,0.665206983690623,2.99561895616294));
#25402=CARTESIAN_POINT('Ctrl Pts',(-0.170490360446883,0.672457732793656,
2.98139101419695));
#25403=CARTESIAN_POINT('Ctrl Pts',(-0.174645209526944,0.689714125571452,
2.95482825180595));
#25404=CARTESIAN_POINT('Ctrl Pts',(-0.177053154990374,0.699719787441729,
2.9424934277131));
#25405=CARTESIAN_POINT('Ctrl Pts',(-0.180063411180702,0.712235629767469,
2.92962121790888));
#25406=CARTESIAN_POINT('Ctrl Pts',(-0.180677622653932,0.7147896798453,2.92710779980363));
#25407=CARTESIAN_POINT('Ctrl Pts',(-0.181315643661013,0.717443124828577,
2.9246182449626));
#25408=CARTESIAN_POINT('Origin',(-0.200268840560683,0.877435120963641,3.1));
#25409=CARTESIAN_POINT('',(-0.147927155402546,0.725063829393324,3.2753817550374));
#25410=CARTESIAN_POINT('',(-0.164665491127673,0.72144665501455,3.27639564195297));
#25411=CARTESIAN_POINT('Ctrl Pts',(-0.147927155402546,0.725063829393324,
3.2753817550374));
#25412=CARTESIAN_POINT('Ctrl Pts',(-0.15362743999372,0.723900860216854,
3.27607258736419));
#25413=CARTESIAN_POINT('Ctrl Pts',(-0.159249892010252,0.722682730173014,
3.27639564195297));
#25414=CARTESIAN_POINT('Ctrl Pts',(-0.164665491127673,0.72144665501455,
3.27639564195297));
#25415=CARTESIAN_POINT('Ctrl Pts',(-0.147927155402546,0.725063829393324,
2.9246182449626));
#25416=CARTESIAN_POINT('Ctrl Pts',(-0.147350705836107,0.722396331130512,
2.92710779980363));
#25417=CARTESIAN_POINT('Ctrl Pts',(-0.146795930454133,0.719828715152708,
2.92962121790888));
#25418=CARTESIAN_POINT('Ctrl Pts',(-0.144077657099531,0.70724622965008,
2.9424934277131));
#25419=CARTESIAN_POINT('Ctrl Pts',(-0.141905847013067,0.697186671420937,
2.95482825180595));
#25420=CARTESIAN_POINT('Ctrl Pts',(-0.138161968462924,0.679836477301521,
2.98139101419695));
#25421=CARTESIAN_POINT('Ctrl Pts',(-0.136589802889265,0.672545867981452,
2.99561895616294));
#25422=CARTESIAN_POINT('Ctrl Pts',(-0.134226872204734,0.661585285903343,
3.02268687665294));
#25423=CARTESIAN_POINT('Ctrl Pts',(-0.133218414707291,0.656905422394462,
3.03802055188041));
#25424=CARTESIAN_POINT('Ctrl Pts',(-0.131905667031906,0.65081257643024,
3.06935267774138));
#25425=CARTESIAN_POINT('Ctrl Pts',(-0.13160133011514,0.649399607261912,
3.08535112900039));
#25426=CARTESIAN_POINT('Ctrl Pts',(-0.13160133011514,0.649399607261913,
3.11464887099961));
#25427=CARTESIAN_POINT('Ctrl Pts',(-0.131905667031905,0.650812576430241,
3.13064732225863));
#25428=CARTESIAN_POINT('Ctrl Pts',(-0.13321841470729,0.656905422394463,
3.16197944811959));
#25429=CARTESIAN_POINT('Ctrl Pts',(-0.134226872204734,0.661585285903343,
3.17731312334706));
#25430=CARTESIAN_POINT('Ctrl Pts',(-0.136589802889265,0.672545867981452,
3.20438104383706));
#25431=CARTESIAN_POINT('Ctrl Pts',(-0.138161968462923,0.679836477301522,
3.21860898580305));
#25432=CARTESIAN_POINT('Ctrl Pts',(-0.141905847013066,0.697186671420939,
3.24517174819405));
#25433=CARTESIAN_POINT('Ctrl Pts',(-0.144077657099534,0.707246229650079,
3.2575065722869));
#25434=CARTESIAN_POINT('Ctrl Pts',(-0.146795930454136,0.719828715152707,
3.27037878209112));
#25435=CARTESIAN_POINT('Ctrl Pts',(-0.147350705836107,0.722396331130512,
3.27289220019637));
#25436=CARTESIAN_POINT('Ctrl Pts',(-0.147927155402546,0.725063829393324,
3.2753817550374));
#25437=CARTESIAN_POINT('',(-0.200268840560683,0.877435120963641,2.86185));
#25438=CARTESIAN_POINT('Origin',(-0.200268840560683,0.877435120963641,3.1));
#25439=CARTESIAN_POINT('Ctrl Pts',(-0.164665491127673,0.72144665501455,
3.27639564195297));
#25440=CARTESIAN_POINT('Ctrl Pts',(-0.170081090245093,0.720210579856085,
3.27639564195297));
#25441=CARTESIAN_POINT('Ctrl Pts',(-0.175675271291417,0.7188685865987,3.27607258736419));
#25442=CARTESIAN_POINT('Ctrl Pts',(-0.181315643661013,0.717443124828577,
3.2753817550374));
#25443=CARTESIAN_POINT('',(-0.200268840560683,0.877435120963641,3.33815));
#25444=CARTESIAN_POINT('Origin',(-0.200268840560683,0.877435120963641,3.1));
#25445=CARTESIAN_POINT('Ctrl Pts',(-0.215847310465459,1.03779089346786,
3.2753817550374));
#25446=CARTESIAN_POINT('Ctrl Pts',(-0.216428786478488,1.04045706470235,
3.27289236009202));
#25447=CARTESIAN_POINT('Ctrl Pts',(-0.21698853610412,1.04302337738549,3.27037910645452));
#25448=CARTESIAN_POINT('Ctrl Pts',(-0.219731899742916,1.0556000331769,3.25750707214144));
#25449=CARTESIAN_POINT('Ctrl Pts',(-0.221925908848716,1.06565456633392,
3.24517226455888));
#25450=CARTESIAN_POINT('Ctrl Pts',(-0.225710868823508,1.08299544455179,
3.21860957458692));
#25451=CARTESIAN_POINT('Ctrl Pts',(-0.22730176616715,1.09028179832403,3.2043816902577));
#25452=CARTESIAN_POINT('Ctrl Pts',(-0.229693765171487,1.10123587450717,
3.17731372034463));
#25453=CARTESIAN_POINT('Ctrl Pts',(-0.230715267060289,1.10591284181213,
3.16197991083841));
#25454=CARTESIAN_POINT('Ctrl Pts',(-0.232045259247275,1.11200185116341,
3.13064753590579));
#25455=CARTESIAN_POINT('Ctrl Pts',(-0.232353729184197,1.11341389632706,
3.11464897022091));
#25456=CARTESIAN_POINT('Ctrl Pts',(-0.232353729184197,1.11341389632706,
3.1));
#25457=CARTESIAN_POINT('Ctrl Pts',(-0.232353729184197,1.11341389632706,
3.08535102977909));
#25458=CARTESIAN_POINT('Ctrl Pts',(-0.232045259247275,1.11200185116341,
3.06935246409421));
#25459=CARTESIAN_POINT('Ctrl Pts',(-0.230715267060289,1.10591284181213,
3.03802008916159));
#25460=CARTESIAN_POINT('Ctrl Pts',(-0.229693765171487,1.10123587450717,
3.02268627965537));
#25461=CARTESIAN_POINT('Ctrl Pts',(-0.22730176616715,1.09028179832403,2.9956183097423));
#25462=CARTESIAN_POINT('Ctrl Pts',(-0.225710868823508,1.08299544455179,
2.98139042541308));
#25463=CARTESIAN_POINT('Ctrl Pts',(-0.221925908848717,1.06565456633392,
2.95482773544113));
#25464=CARTESIAN_POINT('Ctrl Pts',(-0.219731899742916,1.0556000331769,2.94249292785856));
#25465=CARTESIAN_POINT('Ctrl Pts',(-0.216988536104113,1.04302337738546,
2.92962089354545));
#25466=CARTESIAN_POINT('Ctrl Pts',(-0.216428786478487,1.04045706470233,
2.92710763990796));
#25467=CARTESIAN_POINT('Ctrl Pts',(-0.215847310465463,1.03779089346786,
2.9246182449626));
#25468=CARTESIAN_POINT('Origin',(0.,0.,3.1));
#25469=CARTESIAN_POINT('Ctrl Pts',(0.644752300229835,0.84136464826396,2.9246182449626));
#25470=CARTESIAN_POINT('Ctrl Pts',(0.646433000359351,0.843514492555987,
2.92710763990798));
#25471=CARTESIAN_POINT('Ctrl Pts',(0.648050798688572,0.845583794128261,
2.92962089354548));
#25472=CARTESIAN_POINT('Ctrl Pts',(0.655979290360836,0.85572466858529,2.94249292785856));
#25473=CARTESIAN_POINT('Ctrl Pts',(0.662318522702308,0.863831545066573,
2.95482773544112));
#25474=CARTESIAN_POINT('Ctrl Pts',(0.673252578886601,0.877812903896685,
2.98139042541308));
#25475=CARTESIAN_POINT('Ctrl Pts',(0.677847358284485,0.883687417317991,
2.9956183097423));
#25476=CARTESIAN_POINT('Ctrl Pts',(0.684755270452366,0.892518849463665,
3.02268627965537));
#25477=CARTESIAN_POINT('Ctrl Pts',(0.687704871914686,0.8962894383426,3.03802008916159));
#25478=CARTESIAN_POINT('Ctrl Pts',(0.691545075614569,0.901198384221383,
3.06935246409421));
#25479=CARTESIAN_POINT('Ctrl Pts',(0.692435660859824,0.902336752864262,
3.08535102977909));
#25480=CARTESIAN_POINT('Ctrl Pts',(0.692435660859824,0.902336752864262,
3.1));
#25481=CARTESIAN_POINT('Ctrl Pts',(0.692435660859824,0.902336752864262,
3.11464897022091));
#25482=CARTESIAN_POINT('Ctrl Pts',(0.691545075614567,0.901198384221383,
3.13064753590579));
#25483=CARTESIAN_POINT('Ctrl Pts',(0.687704871914685,0.896289438342601,
3.16197991083841));
#25484=CARTESIAN_POINT('Ctrl Pts',(0.684755270452365,0.892518849463665,
3.17731372034463));
#25485=CARTESIAN_POINT('Ctrl Pts',(0.677847358284485,0.883687417317991,
3.2043816902577));
#25486=CARTESIAN_POINT('Ctrl Pts',(0.6732525788866,0.877812903896684,3.21860957458692));
#25487=CARTESIAN_POINT('Ctrl Pts',(0.662318522702307,0.863831545066573,
3.24517226455888));
#25488=CARTESIAN_POINT('Ctrl Pts',(0.655979290360836,0.85572466858529,3.25750707214144));
#25489=CARTESIAN_POINT('Ctrl Pts',(0.648050798688553,0.845583794128237,
3.27037910645455));
#25490=CARTESIAN_POINT('Ctrl Pts',(0.646433000359339,0.843514492555969,
3.27289236009204));
#25491=CARTESIAN_POINT('Ctrl Pts',(0.644752300229836,0.841364648263959,
3.2753817550374));
#25492=CARTESIAN_POINT('Origin',(0.,0.,3.1));
#25493=CARTESIAN_POINT('',(0.447871167131128,0.589076750222415,3.2753817550374));
#25494=CARTESIAN_POINT('Origin',(0.,0.,3.2753817550374));
#25495=CARTESIAN_POINT('Ctrl Pts',(0.447871167131129,0.589076750222414,
3.2753817550374));
#25496=CARTESIAN_POINT('Ctrl Pts',(0.446194419897493,0.586923529425736,
3.27289220019637));
#25497=CARTESIAN_POINT('Ctrl Pts',(0.444580537728585,0.58485089538211,3.27037878209112));
#25498=CARTESIAN_POINT('Ctrl Pts',(0.436672122204367,0.574693882270447,
3.2575065722869));
#25499=CARTESIAN_POINT('Ctrl Pts',(0.430350710191136,0.566572846562107,
3.24517174819405));
#25500=CARTESIAN_POINT('Ctrl Pts',(0.419449625073301,0.552565269832587,
3.21860898580305));
#25501=CARTESIAN_POINT('Ctrl Pts',(0.414869876004012,0.546678794884774,
3.20438104383706));
#25502=CARTESIAN_POINT('Ctrl Pts',(0.407985330685283,0.537828888858988,
3.17731312334706));
#25503=CARTESIAN_POINT('Ctrl Pts',(0.405046225197691,0.534050030841187,
3.16197944811959));
#25504=CARTESIAN_POINT('Ctrl Pts',(0.401219893621934,0.529130146180412,
3.13064732225863));
#25505=CARTESIAN_POINT('Ctrl Pts',(0.400332631188562,0.52798915178784,3.11464887099961));
#25506=CARTESIAN_POINT('Ctrl Pts',(0.400332631188562,0.52798915178784,3.08535112900039));
#25507=CARTESIAN_POINT('Ctrl Pts',(0.401219893621934,0.529130146180412,
3.06935267774138));
#25508=CARTESIAN_POINT('Ctrl Pts',(0.405046225197691,0.534050030841187,
3.03802055188041));
#25509=CARTESIAN_POINT('Ctrl Pts',(0.407985330685283,0.537828888858988,
3.02268687665294));
#25510=CARTESIAN_POINT('Ctrl Pts',(0.414869876004012,0.546678794884774,
2.99561895616294));
#25511=CARTESIAN_POINT('Ctrl Pts',(0.419449625073304,0.552565269832584,
2.98139101419695));
#25512=CARTESIAN_POINT('Ctrl Pts',(0.430350710191138,0.566572846562104,
2.95482825180595));
#25513=CARTESIAN_POINT('Ctrl Pts',(0.436672122204369,0.574693882270445,
2.9424934277131));
#25514=CARTESIAN_POINT('Ctrl Pts',(0.444580537728587,0.584850895382108,
2.92962121790888));
#25515=CARTESIAN_POINT('Ctrl Pts',(0.446194419897493,0.586923529425736,
2.92710779980363));
#25516=CARTESIAN_POINT('Ctrl Pts',(0.447871167131129,0.589076750222414,
2.9246182449626));
#25517=CARTESIAN_POINT('Origin',(0.56114082167286,0.703648334221227,3.1));
#25518=CARTESIAN_POINT('',(0.461382453375463,0.578555297026342,3.27639564195297));
#25519=CARTESIAN_POINT('Ctrl Pts',(0.461382453375463,0.578555297026342,
3.27639564195297));
#25520=CARTESIAN_POINT('Ctrl Pts',(0.457039480081212,0.582018702657134,
3.27639564195297));
#25521=CARTESIAN_POINT('Ctrl Pts',(0.452502352671194,0.585555690407633,
3.27607258736419));
#25522=CARTESIAN_POINT('Ctrl Pts',(0.447871167131128,0.589076750222415,
3.2753817550374));
#25523=CARTESIAN_POINT('',(0.56114082167286,0.703648334221227,3.33815));
#25524=CARTESIAN_POINT('Origin',(0.56114082167286,0.703648334221227,3.1));
#25525=CARTESIAN_POINT('',(0.474646655807069,0.56772401052903,3.2753817550374));
#25526=CARTESIAN_POINT('Ctrl Pts',(0.474646655807069,0.56772401052903,3.2753817550374));
#25527=CARTESIAN_POINT('Ctrl Pts',(0.470183340581477,0.571455573060031,
3.27607258736419));
#25528=CARTESIAN_POINT('Ctrl Pts',(0.465725426669714,0.57509189139555,3.27639564195297));
#25529=CARTESIAN_POINT('Ctrl Pts',(0.461382453375463,0.578555297026342,
3.27639564195297));
#25530=CARTESIAN_POINT('Ctrl Pts',(0.474646655807069,0.56772401052903,2.9246182449626));
#25531=CARTESIAN_POINT('Ctrl Pts',(0.472920532111735,0.565610166146593,
2.92710779980363));
#25532=CARTESIAN_POINT('Ctrl Pts',(0.471258985898383,0.563575542910017,
2.92962121790888));
#25533=CARTESIAN_POINT('Ctrl Pts',(0.46311641831999,0.553605259830511,2.9424934277131));
#25534=CARTESIAN_POINT('Ctrl Pts',(0.45660564043721,0.545635238363898,2.95482825180595));
#25535=CARTESIAN_POINT('Ctrl Pts',(0.44537498254313,0.531890487153134,2.98139101419695));
#25536=CARTESIAN_POINT('Ctrl Pts',(0.440655183852335,0.526115698051596,
2.99561895616294));
#25537=CARTESIAN_POINT('Ctrl Pts',(0.433559118901799,0.517434473303403,
3.02268687665294));
#25538=CARTESIAN_POINT('Ctrl Pts',(0.430529017242168,0.513728182311292,
3.03802055188041));
#25539=CARTESIAN_POINT('Ctrl Pts',(0.426583923237528,0.508903007527151,
3.06935267774138));
#25540=CARTESIAN_POINT('Ctrl Pts',(0.425668970421903,0.507784095477554,
3.08535112900039));
#25541=CARTESIAN_POINT('Ctrl Pts',(0.425668970421903,0.507784095477554,
3.11464887099961));
#25542=CARTESIAN_POINT('Ctrl Pts',(0.426583923237527,0.508903007527151,
3.13064732225863));
#25543=CARTESIAN_POINT('Ctrl Pts',(0.430529017242168,0.513728182311292,
3.16197944811959));
#25544=CARTESIAN_POINT('Ctrl Pts',(0.433559118901799,0.517434473303403,
3.17731312334706));
#25545=CARTESIAN_POINT('Ctrl Pts',(0.440655183852335,0.526115698051596,
3.20438104383706));
#25546=CARTESIAN_POINT('Ctrl Pts',(0.445374982543131,0.531890487153134,
3.21860898580305));
#25547=CARTESIAN_POINT('Ctrl Pts',(0.456605640437211,0.545635238363898,
3.24517174819405));
#25548=CARTESIAN_POINT('Ctrl Pts',(0.463116418319992,0.553605259830509,
3.2575065722869));
#25549=CARTESIAN_POINT('Ctrl Pts',(0.471258985898385,0.563575542910015,
3.27037878209112));
#25550=CARTESIAN_POINT('Ctrl Pts',(0.472920532111735,0.565610166146593,
3.27289220019637));
#25551=CARTESIAN_POINT('Ctrl Pts',(0.474646655807069,0.56772401052903,3.2753817550374));
#25552=CARTESIAN_POINT('',(0.56114082167286,0.703648334221227,2.86185));
#25553=CARTESIAN_POINT('Origin',(0.56114082167286,0.703648334221227,3.1));
#25554=CARTESIAN_POINT('Ctrl Pts',(0.676798995897951,0.815808261267024,
3.2753817550374));
#25555=CARTESIAN_POINT('Ctrl Pts',(0.678520948142572,0.81792520809502,3.27289236009202));
#25556=CARTESIAN_POINT('Ctrl Pts',(0.680178374008934,0.819962907760957,
3.27037910645452));
#25557=CARTESIAN_POINT('Ctrl Pts',(0.688300740199246,0.829949172449061,
3.25750707214144));
#25558=CARTESIAN_POINT('Ctrl Pts',(0.694793748460268,0.837933416726651,
3.24517226455888));
#25559=CARTESIAN_POINT('Ctrl Pts',(0.705991509039914,0.851704478318938,
3.21860957458692));
#25560=CARTESIAN_POINT('Ctrl Pts',(0.710696301541893,0.8574912592173,3.2043816902577));
#25561=CARTESIAN_POINT('Ctrl Pts',(0.717769156177965,0.866191154133894,
3.17731372034463));
#25562=CARTESIAN_POINT('Ctrl Pts',(0.720788860449207,0.869905837888228,
3.16197991083841));
#25563=CARTESIAN_POINT('Ctrl Pts',(0.724720203091942,0.874742102885396,
3.13064753590579));
#25564=CARTESIAN_POINT('Ctrl Pts',(0.725631856595695,0.875863670152773,
3.11464897022091));
#25565=CARTESIAN_POINT('Ctrl Pts',(0.725631856595695,0.875863670152773,
3.1));
#25566=CARTESIAN_POINT('Ctrl Pts',(0.725631856595695,0.875863670152773,
3.08535102977909));
#25567=CARTESIAN_POINT('Ctrl Pts',(0.724720203091943,0.874742102885394,
3.06935246409421));
#25568=CARTESIAN_POINT('Ctrl Pts',(0.720788860449208,0.869905837888227,
3.03802008916159));
#25569=CARTESIAN_POINT('Ctrl Pts',(0.717769156177965,0.866191154133894,
3.02268627965537));
#25570=CARTESIAN_POINT('Ctrl Pts',(0.710696301541893,0.8574912592173,2.9956183097423));
#25571=CARTESIAN_POINT('Ctrl Pts',(0.705991509039915,0.851704478318936,
2.98139042541308));
#25572=CARTESIAN_POINT('Ctrl Pts',(0.69479374846027,0.837933416726649,2.95482773544112));
#25573=CARTESIAN_POINT('Ctrl Pts',(0.688300740199246,0.829949172449061,
2.94249292785856));
#25574=CARTESIAN_POINT('Ctrl Pts',(0.680178374008915,0.819962907760934,
2.92962089354545));
#25575=CARTESIAN_POINT('Ctrl Pts',(0.67852094814256,0.817925208095002,2.92710763990797));
#25576=CARTESIAN_POINT('Ctrl Pts',(0.676798995897952,0.815808261267023,
2.9246182449626));
#25577=CARTESIAN_POINT('Origin',(0.,0.,3.1));
#25578=CARTESIAN_POINT('',(-1.06,-1.29812560709619E-16,2.7));
#25579=CARTESIAN_POINT('',(-1.06,-1.29812560709619E-16,3.1));
#25580=CARTESIAN_POINT('Origin',(0.,0.,2.7));
#25581=CARTESIAN_POINT('Origin',(0.,0.,3.1));
#25582=CARTESIAN_POINT('Ctrl Pts',(1.05980185416667,-0.0204946311236757,
3.2753817550374));
#25583=CARTESIAN_POINT('Ctrl Pts',(1.06253056950731,-0.0205210128414943,
3.27289236009202));
#25584=CARTESIAN_POINT('Ctrl Pts',(1.06515709538297,-0.0205463556027087,
3.27037910645452));
#25585=CARTESIAN_POINT('Ctrl Pts',(1.07802888399501,-0.0206703430107339,
3.25750707214144));
#25586=CARTESIAN_POINT('Ctrl Pts',(1.08831954196908,-0.0207686864025012,
3.24517226455888));
#25587=CARTESIAN_POINT('Ctrl Pts',(1.106067880994,-0.0209373316932479,3.21860957458692));
#25588=CARTESIAN_POINT('Ctrl Pts',(1.11352555862733,-0.0210076877140537,
3.2043816902577));
#25589=CARTESIAN_POINT('Ctrl Pts',(1.12473726310291,-0.0211131723817156,
3.17731372034463));
#25590=CARTESIAN_POINT('Ctrl Pts',(1.12952427462721,-0.0211580048107555,
3.16197991083841));
#25591=CARTESIAN_POINT('Ctrl Pts',(1.13575657090491,-0.0212162903523946,
3.13064753590579));
#25592=CARTESIAN_POINT('Ctrl Pts',(1.13720185416667,-0.0212297640094256,
3.11464897022091));
#25593=CARTESIAN_POINT('Ctrl Pts',(1.13720185416667,-0.0212297640094256,
3.1));
#25594=CARTESIAN_POINT('Ctrl Pts',(1.13720185416667,-0.0212297640094256,
3.08535102977909));
#25595=CARTESIAN_POINT('Ctrl Pts',(1.13575657090491,-0.0212162903523946,
3.06935246409421));
#25596=CARTESIAN_POINT('Ctrl Pts',(1.12952427462721,-0.0211580048107555,
3.03802008916159));
#25597=CARTESIAN_POINT('Ctrl Pts',(1.12473726310291,-0.0211131723817156,
3.02268627965537));
#25598=CARTESIAN_POINT('Ctrl Pts',(1.11352555862733,-0.0210076877140537,
2.9956183097423));
#25599=CARTESIAN_POINT('Ctrl Pts',(1.106067880994,-0.0209373316932489,2.98139042541308));
#25600=CARTESIAN_POINT('Ctrl Pts',(1.08831954196908,-0.020768686402502,
2.95482773544113));
#25601=CARTESIAN_POINT('Ctrl Pts',(1.07802888399501,-0.0206703430107339,
2.94249292785856));
#25602=CARTESIAN_POINT('Ctrl Pts',(1.06515709538294,-0.0205463556027084,
2.92962089354545));
#25603=CARTESIAN_POINT('Ctrl Pts',(1.06253056950729,-0.0205210128414896,
2.92710763990796));
#25604=CARTESIAN_POINT('Ctrl Pts',(1.05980185416667,-0.0204946311236712,
2.9246182449626));
#25605=CARTESIAN_POINT('Origin',(0.,0.,3.1));
#25606=CARTESIAN_POINT('',(-0.74,-9.06238631369041E-17,3.5));
#25607=CARTESIAN_POINT('Origin',(0.,0.,3.5));
#25608=CARTESIAN_POINT('',(-0.74,-9.06238631369041E-17,3.1));
#25609=CARTESIAN_POINT('',(0.739801854166667,-0.0171235677229433,3.2753817550374));
#25610=CARTESIAN_POINT('Origin',(0.,0.,3.2753817550374));
#25611=CARTESIAN_POINT('',(0.74,-1.41339830831208E-17,3.27639564195297));
#25612=CARTESIAN_POINT('Ctrl Pts',(0.739801854166667,-0.0171235677229433,
3.2753817550374));
#25613=CARTESIAN_POINT('Ctrl Pts',(0.739936475706564,-0.0113074161803182,
3.27607258736419));
#25614=CARTESIAN_POINT('Ctrl Pts',(0.74,-0.00555487133946258,3.27639564195297));
#25615=CARTESIAN_POINT('Ctrl Pts',(0.74,-8.67361737988404E-18,3.27639564195297));
#25616=CARTESIAN_POINT('',(0.739801854166667,0.0171235677229433,3.2753817550374));
#25617=CARTESIAN_POINT('Ctrl Pts',(0.74,-8.67361737988404E-18,3.27639564195297));
#25618=CARTESIAN_POINT('Ctrl Pts',(0.74,0.0055548713394626,3.27639564195297));
#25619=CARTESIAN_POINT('Ctrl Pts',(0.739936475706564,0.0113074161803183,
3.27607258736419));
#25620=CARTESIAN_POINT('Ctrl Pts',(0.739801854166667,0.0171235677229433,
3.2753817550374));
#25621=CARTESIAN_POINT('Origin',(0.,0.,3.2753817550374));
#25622=CARTESIAN_POINT('Origin',(0.,0.,3.1));
#25623=CARTESIAN_POINT('Ctrl Pts',(0.739801854166667,-0.0171235677229416,
2.9246182449626));
#25624=CARTESIAN_POINT('Ctrl Pts',(0.737072963558652,-0.0170919902904609,
2.92710779980363));
#25625=CARTESIAN_POINT('Ctrl Pts',(0.734446273937994,-0.017061507989918,
2.92962121790888));
#25626=CARTESIAN_POINT('Ctrl Pts',(0.721574384891244,-0.0169117621307234,
2.9424934277131));
#25627=CARTESIAN_POINT('Ctrl Pts',(0.711283767580619,-0.0167906581116384,
2.95482825180595));
#25628=CARTESIAN_POINT('Ctrl Pts',(0.69353548770023,-0.0165798884102157,
2.98139101419695));
#25629=CARTESIAN_POINT('Ctrl Pts',(0.686077829425498,-0.0164903233155346,
2.99561895616294));
#25630=CARTESIAN_POINT('Ctrl Pts',(0.674866250480993,-0.0163550514337092,
3.02268687665294));
#25631=CARTESIAN_POINT('Ctrl Pts',(0.670079318016798,-0.0162968571974327,
3.03802055188041));
#25632=CARTESIAN_POINT('Ctrl Pts',(0.663847118582878,-0.0162209057734067,
3.06935267774138));
#25633=CARTESIAN_POINT('Ctrl Pts',(0.662401854166667,-0.0162031971092804,
3.08535112900039));
#25634=CARTESIAN_POINT('Ctrl Pts',(0.662401854166667,-0.0162031971092804,
3.11464887099961));
#25635=CARTESIAN_POINT('Ctrl Pts',(0.663847118582878,-0.0162209057734067,
3.13064732225863));
#25636=CARTESIAN_POINT('Ctrl Pts',(0.670079318016799,-0.0162968571974327,
3.16197944811959));
#25637=CARTESIAN_POINT('Ctrl Pts',(0.674866250480993,-0.0163550514337092,
3.17731312334706));
#25638=CARTESIAN_POINT('Ctrl Pts',(0.686077829425498,-0.0164903233155346,
3.20438104383706));
#25639=CARTESIAN_POINT('Ctrl Pts',(0.693535487700231,-0.0165798884102181,
3.21860898580305));
#25640=CARTESIAN_POINT('Ctrl Pts',(0.71128376758062,-0.0167906581116409,
3.24517174819405));
#25641=CARTESIAN_POINT('Ctrl Pts',(0.721574384891244,-0.0169117621307202,
3.2575065722869));
#25642=CARTESIAN_POINT('Ctrl Pts',(0.734446273937994,-0.0170615079899147,
3.27037878209112));
#25643=CARTESIAN_POINT('Ctrl Pts',(0.737072963558652,-0.0170919902904609,
3.27289220019637));
#25644=CARTESIAN_POINT('Ctrl Pts',(0.739801854166667,-0.0171235677229416,
3.2753817550374));
#25645=CARTESIAN_POINT('Origin',(0.9,0.,3.1));
#25646=CARTESIAN_POINT('',(0.9,-1.78583896120461E-33,2.86185));
#25647=CARTESIAN_POINT('Origin',(0.9,0.,3.1));
#25648=CARTESIAN_POINT('Ctrl Pts',(0.739801854166667,0.0171235677229416,
3.2753817550374));
#25649=CARTESIAN_POINT('Ctrl Pts',(0.737072963558652,0.0170919902904609,
3.27289220019637));
#25650=CARTESIAN_POINT('Ctrl Pts',(0.734446273937994,0.0170615079899147,
3.27037878209112));
#25651=CARTESIAN_POINT('Ctrl Pts',(0.721574384891244,0.0169117621307202,
3.2575065722869));
#25652=CARTESIAN_POINT('Ctrl Pts',(0.71128376758062,0.0167906581116409,
3.24517174819405));
#25653=CARTESIAN_POINT('Ctrl Pts',(0.693535487700231,0.0165798884102181,
3.21860898580305));
#25654=CARTESIAN_POINT('Ctrl Pts',(0.686077829425498,0.0164903233155346,
3.20438104383706));
#25655=CARTESIAN_POINT('Ctrl Pts',(0.674866250480993,0.0163550514337092,
3.17731312334706));
#25656=CARTESIAN_POINT('Ctrl Pts',(0.670079318016799,0.0162968571974327,
3.16197944811959));
#25657=CARTESIAN_POINT('Ctrl Pts',(0.663847118582878,0.0162209057734067,
3.13064732225863));
#25658=CARTESIAN_POINT('Ctrl Pts',(0.662401854166667,0.0162031971092804,
3.11464887099961));
#25659=CARTESIAN_POINT('Ctrl Pts',(0.662401854166667,0.0162031971092804,
3.08535112900039));
#25660=CARTESIAN_POINT('Ctrl Pts',(0.663847118582878,0.0162209057734067,
3.06935267774138));
#25661=CARTESIAN_POINT('Ctrl Pts',(0.670079318016798,0.0162968571974327,
3.03802055188041));
#25662=CARTESIAN_POINT('Ctrl Pts',(0.674866250480993,0.0163550514337092,
3.02268687665294));
#25663=CARTESIAN_POINT('Ctrl Pts',(0.686077829425498,0.0164903233155346,
2.99561895616294));
#25664=CARTESIAN_POINT('Ctrl Pts',(0.69353548770023,0.0165798884102157,
2.98139101419695));
#25665=CARTESIAN_POINT('Ctrl Pts',(0.711283767580619,0.0167906581116384,
2.95482825180595));
#25666=CARTESIAN_POINT('Ctrl Pts',(0.721574384891244,0.0169117621307234,
2.9424934277131));
#25667=CARTESIAN_POINT('Ctrl Pts',(0.734446273937994,0.017061507989918,
2.92962121790888));
#25668=CARTESIAN_POINT('Ctrl Pts',(0.737072963558652,0.0170919902904609,
2.92710779980363));
#25669=CARTESIAN_POINT('Ctrl Pts',(0.739801854166667,0.0171235677229416,
2.9246182449626));
#25670=CARTESIAN_POINT('',(0.9,-1.78583896120461E-33,3.33815));
#25671=CARTESIAN_POINT('Origin',(0.9,0.,3.1));
#25672=CARTESIAN_POINT('Ctrl Pts',(1.05980185416667,0.0204946311236712,
2.9246182449626));
#25673=CARTESIAN_POINT('Ctrl Pts',(1.06253056950731,0.0205210128414899,
2.92710763990798));
#25674=CARTESIAN_POINT('Ctrl Pts',(1.06515709538297,0.0205463556027087,
2.92962089354548));
#25675=CARTESIAN_POINT('Ctrl Pts',(1.07802888399501,0.0206703430107339,
2.94249292785856));
#25676=CARTESIAN_POINT('Ctrl Pts',(1.08831954196908,0.0207686864025012,
2.95482773544112));
#25677=CARTESIAN_POINT('Ctrl Pts',(1.106067880994,0.0209373316932479,2.98139042541308));
#25678=CARTESIAN_POINT('Ctrl Pts',(1.11352555862733,0.0210076877140537,
2.9956183097423));
#25679=CARTESIAN_POINT('Ctrl Pts',(1.12473726310291,0.0211131723817156,
3.02268627965537));
#25680=CARTESIAN_POINT('Ctrl Pts',(1.12952427462721,0.0211580048107574,
3.03802008916159));
#25681=CARTESIAN_POINT('Ctrl Pts',(1.13575657090491,0.0212162903523964,
3.06935246409421));
#25682=CARTESIAN_POINT('Ctrl Pts',(1.13720185416667,0.0212297640094256,
3.08535102977909));
#25683=CARTESIAN_POINT('Ctrl Pts',(1.13720185416667,0.0212297640094256,
3.1));
#25684=CARTESIAN_POINT('Ctrl Pts',(1.13720185416667,0.0212297640094256,
3.11464897022091));
#25685=CARTESIAN_POINT('Ctrl Pts',(1.13575657090491,0.0212162903523946,
3.13064753590579));
#25686=CARTESIAN_POINT('Ctrl Pts',(1.12952427462721,0.0211580048107555,
3.16197991083841));
#25687=CARTESIAN_POINT('Ctrl Pts',(1.12473726310291,0.0211131723817156,
3.17731372034463));
#25688=CARTESIAN_POINT('Ctrl Pts',(1.11352555862733,0.0210076877140537,
3.2043816902577));
#25689=CARTESIAN_POINT('Ctrl Pts',(1.106067880994,0.0209373316932487,3.21860957458692));
#25690=CARTESIAN_POINT('Ctrl Pts',(1.08831954196908,0.0207686864025019,
3.24517226455888));
#25691=CARTESIAN_POINT('Ctrl Pts',(1.07802888399501,0.0206703430107339,
3.25750707214144));
#25692=CARTESIAN_POINT('Ctrl Pts',(1.06515709538294,0.0205463556027084,
3.27037910645455));
#25693=CARTESIAN_POINT('Ctrl Pts',(1.06253056950729,0.0205210128414941,
3.27289236009204));
#25694=CARTESIAN_POINT('Ctrl Pts',(1.05980185416667,0.0204946311236757,
3.2753817550374));
#25695=CARTESIAN_POINT('Origin',(0.,0.,3.1));
#25696=CARTESIAN_POINT('Origin',(1.27,0.,2.7));
#25697=CARTESIAN_POINT('',(-1.27,-1.55530143491714E-16,2.7));
#25698=CARTESIAN_POINT('Origin',(0.,0.,2.7));
#25699=CARTESIAN_POINT('Origin',(0.,0.,2.715));
#25700=CARTESIAN_POINT('',(-1.3,-1.59204083889156E-16,2.73));
#25701=CARTESIAN_POINT('Origin',(0.,0.,2.73));
#25702=CARTESIAN_POINT('',(-1.285,-1.57367113690435E-16,2.715));
#25703=CARTESIAN_POINT('Origin',(0.,0.,3.1));
#25704=CARTESIAN_POINT('',(-1.3,-1.59204083889156E-16,3.47));
#25705=CARTESIAN_POINT('Origin',(0.,0.,3.47));
#25706=CARTESIAN_POINT('',(-1.3,-1.59204083889156E-16,3.1));
#25707=CARTESIAN_POINT('Origin',(0.,0.,3.485));
#25708=CARTESIAN_POINT('',(-1.27,-1.55530143491714E-16,3.5));
#25709=CARTESIAN_POINT('Origin',(0.,0.,3.5));
#25710=CARTESIAN_POINT('',(-1.285,-1.57367113690435E-16,3.485));
#25711=CARTESIAN_POINT('Origin',(1.06,0.,3.5));
#25712=CARTESIAN_POINT('Origin',(0.,0.,3.1));
#25713=CARTESIAN_POINT('Origin',(0.,0.,3.1));
#25714=CARTESIAN_POINT('',(-0.5,-6.12323399573677E-17,3.47));
#25715=CARTESIAN_POINT('Origin',(0.,0.,3.47));
#25716=CARTESIAN_POINT('',(-0.5,-6.12323399573677E-17,2.73));
#25717=CARTESIAN_POINT('',(-0.5,-6.12323399573677E-17,3.1));
#25718=CARTESIAN_POINT('Origin',(0.,0.,2.73));
#25719=CARTESIAN_POINT('Origin',(0.,0.,2.715));
#25720=CARTESIAN_POINT('',(-0.53,-6.49062803548097E-17,2.7));
#25721=CARTESIAN_POINT('',(-0.515,-6.30693101560887E-17,2.715));
#25722=CARTESIAN_POINT('Origin',(0.,0.,2.7));
#25723=CARTESIAN_POINT('Origin',(0.74,0.,2.7));
#25724=CARTESIAN_POINT('Origin',(0.53,0.,3.5));
#25725=CARTESIAN_POINT('',(-0.53,-6.49062803548097E-17,3.5));
#25726=CARTESIAN_POINT('Origin',(0.,0.,3.5));
#25727=CARTESIAN_POINT('Origin',(0.,0.,3.485));
#25728=CARTESIAN_POINT('',(-0.515,-6.30693101560887E-17,3.485));
#25729=CARTESIAN_POINT('',(0.,0.,0.));
#25730=CARTESIAN_POINT('Origin',(0.,0.,2.65));
#25731=CARTESIAN_POINT('',(-0.5,-6.12323399573677E-17,2.7));
#25732=CARTESIAN_POINT('Origin',(0.,0.,2.7));
#25733=CARTESIAN_POINT('',(-0.5,-6.12323399573677E-17,2.6));
#25734=CARTESIAN_POINT('',(-0.5,-6.12323399573677E-17,2.65));
#25735=CARTESIAN_POINT('Origin',(0.,0.,2.6));
#25736=CARTESIAN_POINT('Origin',(0.8,0.,2.6));
#25737=CARTESIAN_POINT('',(-0.8,-9.79717439317883E-17,2.6));
#25738=CARTESIAN_POINT('Origin',(0.,0.,2.6));
#25739=CARTESIAN_POINT('Origin',(0.,0.,2.65));
#25740=CARTESIAN_POINT('',(-0.8,-9.79717439317883E-17,2.7));
#25741=CARTESIAN_POINT('Origin',(0.,0.,2.7));
#25742=CARTESIAN_POINT('',(-0.8,-9.79717439317883E-17,2.65));
#25743=CARTESIAN_POINT('Origin',(0.5,0.,2.7));
#25744=CARTESIAN_POINT('',(0.,0.,0.));
#25745=CARTESIAN_POINT('Origin',(0.35,0.16,5.76));
#25746=CARTESIAN_POINT('',(0.79,0.17,5.75));
#25747=CARTESIAN_POINT('',(0.79,0.15,5.77));
#25748=CARTESIAN_POINT('',(0.79,0.16,5.76));
#25749=CARTESIAN_POINT('',(0.45596052460712,0.15,5.77));
#25750=CARTESIAN_POINT('',(0.35,0.15,5.77));
#25751=CARTESIAN_POINT('',(0.448887513749269,0.17,5.75));
#25752=CARTESIAN_POINT('Origin',(0.,0.,5.92));
#25753=CARTESIAN_POINT('',(0.35,0.17,5.75));
#25754=CARTESIAN_POINT('Origin',(0.7,0.15,5.75));
#25755=CARTESIAN_POINT('',(0.79,0.15,5.83));
#25756=CARTESIAN_POINT('',(0.79,0.15,5.75));
#25757=CARTESIAN_POINT('',(0.45596052460712,0.15,5.83));
#25758=CARTESIAN_POINT('',(0.35,0.15,5.83));
#25759=CARTESIAN_POINT('',(0.45596052460712,0.15,5.75));
#25760=CARTESIAN_POINT('Origin',(0.79,0.15,5.75));
#25761=CARTESIAN_POINT('',(0.79,0.4,5.75));
#25762=CARTESIAN_POINT('',(0.79,0.15,5.75));
#25763=CARTESIAN_POINT('',(0.79,0.4,5.85));
#25764=CARTESIAN_POINT('',(0.79,0.4,5.75));
#25765=CARTESIAN_POINT('',(0.79,0.17,5.85));
#25766=CARTESIAN_POINT('',(0.79,0.15,5.85));
#25767=CARTESIAN_POINT('',(0.79,0.135,5.815));
#25768=CARTESIAN_POINT('Origin',(0.19,-0.16,5.76));
#25769=CARTESIAN_POINT('',(0.79,-0.15,5.77));
#25770=CARTESIAN_POINT('',(0.79,-0.17,5.75));
#25771=CARTESIAN_POINT('',(0.79,-0.222500000000001,5.6975));
#25772=CARTESIAN_POINT('',(0.448887513749269,-0.17,5.75));
#25773=CARTESIAN_POINT('',(0.19,-0.17,5.75));
#25774=CARTESIAN_POINT('',(0.45596052460712,-0.15,5.77));
#25775=CARTESIAN_POINT('Origin',(0.,0.,5.92));
#25776=CARTESIAN_POINT('',(0.19,-0.15,5.77));
#25777=CARTESIAN_POINT('Origin',(0.38,-0.15,5.75));
#25778=CARTESIAN_POINT('',(0.45596052460712,-0.15,5.83));
#25779=CARTESIAN_POINT('',(0.45596052460712,-0.15,5.75));
#25780=CARTESIAN_POINT('',(0.79,-0.15,5.83));
#25781=CARTESIAN_POINT('',(0.19,-0.15,5.83));
#25782=CARTESIAN_POINT('',(0.79,-0.15,5.75));
#25783=CARTESIAN_POINT('Origin',(0.,0.,5.75));
#25784=CARTESIAN_POINT('',(0.448887513749269,0.17,5.85));
#25785=CARTESIAN_POINT('Origin',(0.,0.,5.68));
#25786=CARTESIAN_POINT('',(0.448887513749269,-0.17,5.85));
#25787=CARTESIAN_POINT('Origin',(0.,0.,5.85));
#25788=CARTESIAN_POINT('Origin',(0.,0.,5.68));
#25789=CARTESIAN_POINT('Origin',(0.,0.,5.75));
#25790=CARTESIAN_POINT('Origin',(0.35,0.16,5.84));
#25791=CARTESIAN_POINT('',(0.35,0.17,5.85));
#25792=CARTESIAN_POINT('Origin',(0.,0.,5.85));
#25793=CARTESIAN_POINT('',(0.55,0.4,5.85));
#25794=CARTESIAN_POINT('',(0.79,0.4,5.85));
#25795=CARTESIAN_POINT('',(0.55,0.239791576165636,5.85));
#25796=CARTESIAN_POINT('',(0.55,0.4,5.85));
#25797=CARTESIAN_POINT('',(0.55,-0.239791576165636,5.85));
#25798=CARTESIAN_POINT('Origin',(0.,0.,5.85));
#25799=CARTESIAN_POINT('',(0.55,-0.4,5.85));
#25800=CARTESIAN_POINT('',(0.55,-0.4,5.85));
#25801=CARTESIAN_POINT('',(0.79,-0.4,5.85));
#25802=CARTESIAN_POINT('',(0.79,-0.4,5.85));
#25803=CARTESIAN_POINT('',(0.79,-0.17,5.85));
#25804=CARTESIAN_POINT('',(0.79,-0.15,5.85));
#25805=CARTESIAN_POINT('',(0.19,-0.17,5.85));
#25806=CARTESIAN_POINT('',(0.65,-0.275,5.85));
#25807=CARTESIAN_POINT('Origin',(0.7,-0.275,5.85));
#25808=CARTESIAN_POINT('',(0.65,0.275,5.85));
#25809=CARTESIAN_POINT('Origin',(0.7,0.275,5.85));
#25810=CARTESIAN_POINT('Origin',(0.19,-0.16,5.84));
#25811=CARTESIAN_POINT('',(0.79,-0.197500000000001,5.8775));
#25812=CARTESIAN_POINT('Origin',(0.79,-0.4,5.75));
#25813=CARTESIAN_POINT('',(0.79,-0.4,5.75));
#25814=CARTESIAN_POINT('',(0.79,-0.4,5.75));
#25815=CARTESIAN_POINT('',(0.79,-0.15,5.75));
#25816=CARTESIAN_POINT('Origin',(0.7,0.275,5.75));
#25817=CARTESIAN_POINT('',(0.65,0.275,5.75));
#25818=CARTESIAN_POINT('Origin',(0.7,0.275,5.75));
#25819=CARTESIAN_POINT('',(0.65,0.275,5.75));
#25820=CARTESIAN_POINT('Origin',(0.7,-0.275,5.75));
#25821=CARTESIAN_POINT('',(0.65,-0.275,5.75));
#25822=CARTESIAN_POINT('Origin',(0.7,-0.275,5.75));
#25823=CARTESIAN_POINT('',(0.65,-0.275,5.75));
#25824=CARTESIAN_POINT('Origin',(0.55,-0.15,5.75));
#25825=CARTESIAN_POINT('',(0.55,-0.239791576165636,5.75));
#25826=CARTESIAN_POINT('',(0.55,-0.239791576165636,5.75));
#25827=CARTESIAN_POINT('',(0.55,-0.4,5.75));
#25828=CARTESIAN_POINT('',(0.55,-0.4,5.75));
#25829=CARTESIAN_POINT('',(0.55,-0.4,5.75));
#25830=CARTESIAN_POINT('Origin',(0.55,-0.4,5.75));
#25831=CARTESIAN_POINT('',(0.79,-0.4,5.75));
#25832=CARTESIAN_POINT('Origin',(0.55,0.4,5.75));
#25833=CARTESIAN_POINT('',(0.55,0.239791576165636,5.75));
#25834=CARTESIAN_POINT('',(0.55,0.239791576165636,5.75));
#25835=CARTESIAN_POINT('',(0.55,0.4,5.75));
#25836=CARTESIAN_POINT('',(0.55,0.4,5.75));
#25837=CARTESIAN_POINT('',(0.55,0.4,5.75));
#25838=CARTESIAN_POINT('Origin',(0.79,0.4,5.75));
#25839=CARTESIAN_POINT('',(0.79,0.4,5.75));
#25840=CARTESIAN_POINT('Origin',(0.,0.,5.75));
#25841=CARTESIAN_POINT('Origin',(0.,0.,5.75));
#25842=CARTESIAN_POINT('Origin',(0.,0.,5.75));
#25843=CARTESIAN_POINT('',(0.,0.,0.));
#25844=CARTESIAN_POINT('Origin',(0.7225,0.,2.35));
#25845=CARTESIAN_POINT('',(0.902013030787577,0.000156006175312973,2.15447233455283));
#25846=CARTESIAN_POINT('',(0.912186969212423,0.000188656559950066,2.15445617438948));
#25847=CARTESIAN_POINT('',(0.7225,-2.39295984553393E-17,2.1546));
#25848=CARTESIAN_POINT('',(0.9246,0.175480723124223,2.43625468886433));
#25849=CARTESIAN_POINT('Ctrl Pts',(0.902013030787577,0.000156006175312973,
2.15447233455283));
#25850=CARTESIAN_POINT('Ctrl Pts',(0.902605775122933,0.0105315582112279,
2.15438573053182));
#25851=CARTESIAN_POINT('Ctrl Pts',(0.90319851945829,0.0208939809769666,
2.15514242031383));
#25852=CARTESIAN_POINT('Ctrl Pts',(0.903791263793647,0.0311127383116308,
2.1567873079189));
#25853=CARTESIAN_POINT('Ctrl Pts',(0.90744260916311,0.0940609776282298,
2.16691992729932));
#25854=CARTESIAN_POINT('Ctrl Pts',(0.911093954532574,0.151557625733869,
2.21075648930218));
#25855=CARTESIAN_POINT('Ctrl Pts',(0.914745299902037,0.178037552885034,
2.26877728473645));
#25856=CARTESIAN_POINT('Ctrl Pts',(0.918030199934691,0.201859981267461,
2.32097517168809));
#25857=CARTESIAN_POINT('Ctrl Pts',(0.921315099967346,0.20057890417809,2.38465312392714));
#25858=CARTESIAN_POINT('Ctrl Pts',(0.9246,0.175579315085691,2.4363567917616));
#25859=CARTESIAN_POINT('',(0.9246,0.175382131162755,2.26384741403295));
#25860=CARTESIAN_POINT('Origin',(0.9246,0.,2.35));
#25861=CARTESIAN_POINT('Ctrl Pts',(0.9246,0.175382131162755,2.26384741403295));
#25862=CARTESIAN_POINT('Ctrl Pts',(0.920948654630537,0.147146138548361,
2.20636697389733));
#25863=CARTESIAN_POINT('Ctrl Pts',(0.917297309261073,0.0887096319793009,
2.16430051430661));
#25864=CARTESIAN_POINT('Ctrl Pts',(0.91364596389161,0.0255879622251572,
2.15600165398185));
#25865=CARTESIAN_POINT('Ctrl Pts',(0.913159632331881,0.0171806336933338,
2.15489630861533));
#25866=CARTESIAN_POINT('Ctrl Pts',(0.912673300772152,0.0086901893208547,
2.15439000799688));
#25867=CARTESIAN_POINT('Ctrl Pts',(0.912186969212423,0.000188656559950066,
2.15445617438948));
#25868=CARTESIAN_POINT('Origin',(0.7225,0.,2.35));
#25869=CARTESIAN_POINT('',(0.832013030787577,-5.13316928911073E-5,2.15488450746355));
#25870=CARTESIAN_POINT('',(0.842186969212423,-2.25216307721818E-5,2.15489585068442));
#25871=CARTESIAN_POINT('',(0.7225,-2.39295984553393E-17,2.1546));
#25872=CARTESIAN_POINT('Ctrl Pts',(0.832013030787577,-5.13316928911073E-5,
2.15488450746355));
#25873=CARTESIAN_POINT('Ctrl Pts',(0.834031036239487,0.0354651555565149,
2.15497065566532));
#25874=CARTESIAN_POINT('Ctrl Pts',(0.836049041691397,0.0710236125991935,
2.16426571469804));
#25875=CARTESIAN_POINT('Ctrl Pts',(0.838067047143308,0.101189284396635,
2.18248793521357));
#25876=CARTESIAN_POINT('Ctrl Pts',(0.841718392512771,0.155770547261944,
2.21545891675267));
#25877=CARTESIAN_POINT('Ctrl Pts',(0.845369737882234,0.192696543426469,
2.27765624603097));
#25878=CARTESIAN_POINT('Ctrl Pts',(0.849021083251698,0.195511659694429,
2.34136106334354));
#25879=CARTESIAN_POINT('Ctrl Pts',(0.852672428621161,0.198326775962389,
2.40506588065611));
#25880=CARTESIAN_POINT('Ctrl Pts',(0.856323773990624,0.167031012333786,
2.47027818600294));
#25881=CARTESIAN_POINT('Ctrl Pts',(0.859975119360087,0.115569820078586,
2.50793461140361));
#25882=CARTESIAN_POINT('Ctrl Pts',(0.86362646472955,0.0641086278233862,
2.54559103680428));
#25883=CARTESIAN_POINT('Ctrl Pts',(0.867277810099014,-0.00751799305840972,
2.55569158225879));
#25884=CARTESIAN_POINT('Ctrl Pts',(0.870929155468477,-0.0673847305716984,
2.53373589439266));
#25885=CARTESIAN_POINT('Ctrl Pts',(0.874580500837941,-0.127251468084987,
2.51178020652652));
#25886=CARTESIAN_POINT('Ctrl Pts',(0.878231846207404,-0.175358322229768,
2.45776828533975));
#25887=CARTESIAN_POINT('Ctrl Pts',(0.881883191576868,-0.190273413583082,
2.39576915322462));
#25888=CARTESIAN_POINT('Ctrl Pts',(0.885534536946331,-0.205188504936396,
2.33377002110949));
#25889=CARTESIAN_POINT('Ctrl Pts',(0.889185882315794,-0.186911833498241,
2.26378367806601));
#25890=CARTESIAN_POINT('Ctrl Pts',(0.892837227685257,-0.143573582515385,
2.21700484492326));
#25891=CARTESIAN_POINT('Ctrl Pts',(0.895895828719363,-0.107270684306657,
2.17781989446053));
#25892=CARTESIAN_POINT('Ctrl Pts',(0.89895442975347,-0.0533825471157545,
2.15491921718409));
#25893=CARTESIAN_POINT('Ctrl Pts',(0.902013030787577,0.000156006175312973,
2.15447233455283));
#25894=CARTESIAN_POINT('Ctrl Pts',(0.912186969212423,0.000188656559950066,
2.15445617438948));
#25895=CARTESIAN_POINT('Ctrl Pts',(0.909021955402688,-0.0551387595903964,
2.15488678092139));
#25896=CARTESIAN_POINT('Ctrl Pts',(0.905856941592954,-0.110935804562971,
2.17956320188895));
#25897=CARTESIAN_POINT('Ctrl Pts',(0.90269192778322,-0.147349415349169,
2.22115976531861));
#25898=CARTESIAN_POINT('Ctrl Pts',(0.899040582413757,-0.189358290230125,
2.2691479980389));
#25899=CARTESIAN_POINT('Ctrl Pts',(0.895389237044293,-0.205569207052808,
2.33965572453828));
#25900=CARTESIAN_POINT('Ctrl Pts',(0.89173789167483,-0.188870701167725,
2.40120859986922));
#25901=CARTESIAN_POINT('Ctrl Pts',(0.888086546305367,-0.172172195282643,
2.46276147520016));
#25902=CARTESIAN_POINT('Ctrl Pts',(0.884435200935903,-0.122564266689796,
2.51535949936266));
#25903=CARTESIAN_POINT('Ctrl Pts',(0.88078385556644,-0.0620996521231525,
2.53558762972075));
#25904=CARTESIAN_POINT('Ctrl Pts',(0.877132510196977,-0.00163503755650911,
2.55581576007883));
#25905=CARTESIAN_POINT('Ctrl Pts',(0.873481164827514,0.06968626298393,2.54367399663249));
#25906=CARTESIAN_POINT('Ctrl Pts',(0.86982981945805,0.120050756860153,2.50456030751575));
#25907=CARTESIAN_POINT('Ctrl Pts',(0.866178474088587,0.170415250736377,
2.465446618399));
#25908=CARTESIAN_POINT('Ctrl Pts',(0.862527128719124,0.199822937948385,
2.39936100361186));
#25909=CARTESIAN_POINT('Ctrl Pts',(0.85887578334966,0.195182096220547,2.33576215814722));
#25910=CARTESIAN_POINT('Ctrl Pts',(0.855224437980197,0.190541254492709,
2.27216331268259));
#25911=CARTESIAN_POINT('Ctrl Pts',(0.851573092610733,0.151851883825026,
2.21105123654046));
#25912=CARTESIAN_POINT('Ctrl Pts',(0.84792174724127,0.096349247276285,2.17965802669765));
#25913=CARTESIAN_POINT('Ctrl Pts',(0.846010154564988,0.0672918936695139,
2.16322270657636));
#25914=CARTESIAN_POINT('Ctrl Pts',(0.844098561888705,0.0336262801083577,
2.15493287481085));
#25915=CARTESIAN_POINT('Ctrl Pts',(0.842186969212423,-2.25216307721818E-5,
2.15489585068442));
#25916=CARTESIAN_POINT('Origin',(0.7225,0.,2.35));
#25917=CARTESIAN_POINT('',(0.762013030787577,-6.2003443803138E-5,2.15432352696516));
#25918=CARTESIAN_POINT('',(0.772186969212424,-9.0396132758989E-5,2.15435402400981));
#25919=CARTESIAN_POINT('',(0.7225,-2.39295984553393E-17,2.1546));
#25920=CARTESIAN_POINT('Ctrl Pts',(0.762013030787577,-6.2003443803138E-5,
2.15432352696516));
#25921=CARTESIAN_POINT('Ctrl Pts',(0.765456297356041,0.0600926660966559,
2.15457840373805));
#25922=CARTESIAN_POINT('Ctrl Pts',(0.768899563924504,0.12046670050001,2.18446056958971));
#25923=CARTESIAN_POINT('Ctrl Pts',(0.772342830492968,0.156551060252226,
2.23256357411178));
#25924=CARTESIAN_POINT('Ctrl Pts',(0.775994175862431,0.194816020943342,
2.28357347396316));
#25925=CARTESIAN_POINT('Ctrl Pts',(0.779645521231895,0.205766923289551,
2.35507294634627));
#25926=CARTESIAN_POINT('Ctrl Pts',(0.783296866601358,0.184523355575946,
2.41519721875575));
#25927=CARTESIAN_POINT('Ctrl Pts',(0.786948211970822,0.163279787862341,
2.47532149116522));
#25928=CARTESIAN_POINT('Ctrl Pts',(0.790599557340285,0.109841750088923,
2.52407056360106));
#25929=CARTESIAN_POINT('Ctrl Pts',(0.794250902709748,0.0480246460538724,
2.53971869511427));
#25930=CARTESIAN_POINT('Ctrl Pts',(0.797902248079211,-0.0137924579811777,
2.55536682662749));
#25931=CARTESIAN_POINT('Ctrl Pts',(0.801553593448674,-0.0839886282778601,
2.53791401721809));
#25932=CARTESIAN_POINT('Ctrl Pts',(0.805204938818138,-0.131279857599735,
2.49513838326637));
#25933=CARTESIAN_POINT('Ctrl Pts',(0.808856284187601,-0.178571086921609,
2.45236274931465));
#25934=CARTESIAN_POINT('Ctrl Pts',(0.812507629557065,-0.202957375268676,
2.38426429082061));
#25935=CARTESIAN_POINT('Ctrl Pts',(0.816158974926528,-0.193570748439729,
2.32119203719827));
#25936=CARTESIAN_POINT('Ctrl Pts',(0.819810320295991,-0.184184121610782,
2.25811978357594));
#25937=CARTESIAN_POINT('Ctrl Pts',(0.823461665665454,-0.141024579605821,
2.20007373482531));
#25938=CARTESIAN_POINT('Ctrl Pts',(0.827113011034917,-0.0833265438202942,
2.17292302734994));
#25939=CARTESIAN_POINT('Ctrl Pts',(0.82874635095247,-0.0575167407266036,
2.1607778233711));
#25940=CARTESIAN_POINT('Ctrl Pts',(0.830379690870024,-0.0287977834434585,
2.15481478054748));
#25941=CARTESIAN_POINT('Ctrl Pts',(0.832013030787577,-5.13316928911073E-5,
2.15488450746355));
#25942=CARTESIAN_POINT('Ctrl Pts',(0.842186969212423,-2.25216307721818E-5,
2.15489585068442));
#25943=CARTESIAN_POINT('Ctrl Pts',(0.840447216519242,-0.0306465108175295,
2.15486215479069));
#25944=CARTESIAN_POINT('Ctrl Pts',(0.838707463826061,-0.0612565748792723,
2.16166420685548));
#25945=CARTESIAN_POINT('Ctrl Pts',(0.836967711132881,-0.0883661713810414,
2.17538290794441));
#25946=CARTESIAN_POINT('Ctrl Pts',(0.833316365763417,-0.145263051059827,
2.20417534257747));
#25947=CARTESIAN_POINT('Ctrl Pts',(0.829665020393954,-0.1867409079876,2.26343455538708));
#25948=CARTESIAN_POINT('Ctrl Pts',(0.82601367502449,-0.194316387043185,
2.32674994840334));
#25949=CARTESIAN_POINT('Ctrl Pts',(0.822362329655027,-0.20189186609877,
2.3900653414196));
#25950=CARTESIAN_POINT('Ctrl Pts',(0.818710984285564,-0.175564967282168,
2.4574369146425));
#25951=CARTESIAN_POINT('Ctrl Pts',(0.815059638916101,-0.127067715562319,
2.49883998978819));
#25952=CARTESIAN_POINT('Ctrl Pts',(0.811408293546638,-0.0785704638424689,
2.54024306493387));
#25953=CARTESIAN_POINT('Ctrl Pts',(0.807756948177174,-0.00790285921937169,
2.55567764200234));
#25954=CARTESIAN_POINT('Ctrl Pts',(0.804105602807711,0.053440578734723,
2.53826485429949));
#25955=CARTESIAN_POINT('Ctrl Pts',(0.800454257438247,0.114784016688818,
2.52085206659665));
#25956=CARTESIAN_POINT('Ctrl Pts',(0.796802912068784,0.16680328797391,2.4705919141225));
#25957=CARTESIAN_POINT('Ctrl Pts',(0.793151566699321,0.186315490867467,
2.40988367637621));
#25958=CARTESIAN_POINT('Ctrl Pts',(0.789500221329858,0.205827693761024,
2.34917543862993));
#25959=CARTESIAN_POINT('Ctrl Pts',(0.785848875960394,0.192832828263045,
2.27801911561151));
#25960=CARTESIAN_POINT('Ctrl Pts',(0.782197530590931,0.153122122420705,
2.22812649775847));
#25961=CARTESIAN_POINT('Ctrl Pts',(0.778860676798095,0.116831712722845,
2.18253114747751));
#25962=CARTESIAN_POINT('Ctrl Pts',(0.775523823005259,0.058229361212525,
2.15469434591714));
#25963=CARTESIAN_POINT('Ctrl Pts',(0.772186969212424,-9.0396132758989E-5,
2.15435402400981));
#25964=CARTESIAN_POINT('Origin',(0.7225,0.,2.35));
#25965=CARTESIAN_POINT('',(0.692013030787577,0.000139690484509278,2.15476836676823));
#25966=CARTESIAN_POINT('',(0.702186969212423,0.000153231897286442,2.15472339864344));
#25967=CARTESIAN_POINT('',(0.7225,-2.39295984553393E-17,2.1546));
#25968=CARTESIAN_POINT('Ctrl Pts',(0.692013030787577,0.000139690484509278,
2.15476836676823));
#25969=CARTESIAN_POINT('Ctrl Pts',(0.693230213103131,0.0215297149542501,
2.15462161982292));
#25970=CARTESIAN_POINT('Ctrl Pts',(0.694447395418685,0.0428763997647126,
2.15787240017079));
#25971=CARTESIAN_POINT('Ctrl Pts',(0.695664577734239,0.0630016027810242,
2.16471549811569));
#25972=CARTESIAN_POINT('Ctrl Pts',(0.699315923103702,0.123373878901117,
2.18524365866698));
#25973=CARTESIAN_POINT('Ctrl Pts',(0.702967268473165,0.172754032575755,
2.23809910815419));
#25974=CARTESIAN_POINT('Ctrl Pts',(0.706618613842629,0.189135076720051,
2.29972604120156));
#25975=CARTESIAN_POINT('Ctrl Pts',(0.710269959212092,0.205516120864348,
2.36135297424894));
#25976=CARTESIAN_POINT('Ctrl Pts',(0.713921304581555,0.188898055478303,
2.43175139085649));
#25977=CARTESIAN_POINT('Ctrl Pts',(0.717572649951018,0.146686965318226,
2.4795472189561));
#25978=CARTESIAN_POINT('Ctrl Pts',(0.721223995320482,0.104475875158149,
2.52734304705571));
#25979=CARTESIAN_POINT('Ctrl Pts',(0.724875340689945,0.0366717602240398,
2.55253628664739));
#25980=CARTESIAN_POINT('Ctrl Pts',(0.728526686059409,-0.0265074936359106,
2.54389920290807));
#25981=CARTESIAN_POINT('Ctrl Pts',(0.732178031428872,-0.0896867474958605,
2.53526211916876));
#25982=CARTESIAN_POINT('Ctrl Pts',(0.735829376798335,-0.148241140281651,
2.49279471209846));
#25983=CARTESIAN_POINT('Ctrl Pts',(0.739480722167799,-0.176075055463372,
2.43542319913709));
#25984=CARTESIAN_POINT('Ctrl Pts',(0.743132067537262,-0.203908970645092,
2.37805168617571));
#25985=CARTESIAN_POINT('Ctrl Pts',(0.746783412906725,-0.201022408222742,
2.30577606732327));
#25986=CARTESIAN_POINT('Ctrl Pts',(0.750434758276188,-0.168701809129991,
2.25080701975543));
#25987=CARTESIAN_POINT('Ctrl Pts',(0.754086103645651,-0.13638121003724,
2.1958379721876));
#25988=CARTESIAN_POINT('Ctrl Pts',(0.757737449015115,-0.0746265742740901,
2.15817549590436));
#25989=CARTESIAN_POINT('Ctrl Pts',(0.761388794384578,-0.0109597468745028,
2.15460442142256));
#25990=CARTESIAN_POINT('Ctrl Pts',(0.761596873185578,-0.00733157266245871,
2.15440091700945));
#25991=CARTESIAN_POINT('Ctrl Pts',(0.761804951986577,-0.00369718859825643,
2.15430812459876));
#25992=CARTESIAN_POINT('Ctrl Pts',(0.762013030787577,-6.2003443803138E-5,
2.15432352696516));
#25993=CARTESIAN_POINT('Ctrl Pts',(0.772186969212424,-9.0396132758989E-5,
2.15435402400981));
#25994=CARTESIAN_POINT('Ctrl Pts',(0.771872477635796,-0.00558691278428774,
2.15432194937309));
#25995=CARTESIAN_POINT('Ctrl Pts',(0.771557986059169,-0.0110809192442294,
2.15453411697643));
#25996=CARTESIAN_POINT('Ctrl Pts',(0.771243494482542,-0.0165534999638003,
2.15499867915844));
#25997=CARTESIAN_POINT('Ctrl Pts',(0.767592149113078,-0.0800918703192643,
2.16039239109913));
#25998=CARTESIAN_POINT('Ctrl Pts',(0.763940803743614,-0.140742064843491,
2.19980872766818));
#25999=CARTESIAN_POINT('Ctrl Pts',(0.760289458374151,-0.171474475734038,
2.25568121175218));
#26000=CARTESIAN_POINT('Ctrl Pts',(0.756638113004688,-0.202206886624584,
2.31155369583617));
#26001=CARTESIAN_POINT('Ctrl Pts',(0.752986767635225,-0.203021513881451,
2.38388232743512));
#26002=CARTESIAN_POINT('Ctrl Pts',(0.749335422265761,-0.173555291090547,
2.44043280991382));
#26003=CARTESIAN_POINT('Ctrl Pts',(0.745684076896298,-0.144089068299643,
2.49698329239251));
#26004=CARTESIAN_POINT('Ctrl Pts',(0.742032731526834,-0.0843419954609685,
2.53775562575096));
#26005=CARTESIAN_POINT('Ctrl Pts',(0.738381386157371,-0.0209412306637257,
2.54457902408615));
#26006=CARTESIAN_POINT('Ctrl Pts',(0.734730040787908,0.0424595341335172,
2.55140242242134));
#26007=CARTESIAN_POINT('Ctrl Pts',(0.731078695418445,0.109513990889328,
2.52427688573327));
#26008=CARTESIAN_POINT('Ctrl Pts',(0.727427350048982,0.150338352188362,
2.47529130523621));
#26009=CARTESIAN_POINT('Ctrl Pts',(0.723776004679519,0.191162713487395,
2.42630572473914));
#26010=CARTESIAN_POINT('Ctrl Pts',(0.720124659310055,0.205756979329652,
2.35546010043307));
#26011=CARTESIAN_POINT('Ctrl Pts',(0.716473313940591,0.187617001058584,
2.29432781126921));
#26012=CARTESIAN_POINT('Ctrl Pts',(0.712821968571128,0.169477022787516,
2.23319552210535));
#26013=CARTESIAN_POINT('Ctrl Pts',(0.709170623201665,0.118602800403123,
2.1817765680837));
#26014=CARTESIAN_POINT('Ctrl Pts',(0.705519277832202,0.0576671708412165,
2.16298655371481));
#26015=CARTESIAN_POINT('Ctrl Pts',(0.704408508292276,0.0391300470238821,
2.15727047552887));
#26016=CARTESIAN_POINT('Ctrl Pts',(0.70329773875235,0.0196618135696035,
2.15457396703312));
#26017=CARTESIAN_POINT('Ctrl Pts',(0.702186969212423,0.000153231897286442,
2.15472339864344));
#26018=CARTESIAN_POINT('Origin',(0.7225,0.,2.35));
#26019=CARTESIAN_POINT('',(0.622013030787577,-0.000161508074393329,2.15467656254574));
#26020=CARTESIAN_POINT('',(0.632186969212423,-0.000152729840347416,2.15472545757722));
#26021=CARTESIAN_POINT('',(0.7225,-2.39295984553393E-17,2.1546));
#26022=CARTESIAN_POINT('Ctrl Pts',(0.622013030787577,-0.000161508074393329,
2.15467656254574));
#26023=CARTESIAN_POINT('Ctrl Pts',(0.624655474219684,0.0462195525262236,
2.15505898169449));
#26024=CARTESIAN_POINT('Ctrl Pts',(0.627297917651792,0.0928466454266734,
2.17165020966846));
#26025=CARTESIAN_POINT('Ctrl Pts',(0.629940361083899,0.127796252092552,
2.2017850173673));
#26026=CARTESIAN_POINT('Ctrl Pts',(0.633591706453363,0.17608984389226,2.2434254889149));
#26027=CARTESIAN_POINT('Ctrl Pts',(0.637243051822826,0.202086571273201,
2.31092592336927));
#26028=CARTESIAN_POINT('Ctrl Pts',(0.640894397192289,0.194200323183497,
2.37420333909549));
#26029=CARTESIAN_POINT('Ctrl Pts',(0.644545742561752,0.186314075093794,
2.43748075482171));
#26030=CARTESIAN_POINT('Ctrl Pts',(0.648197087931216,0.144544851533446,
2.49653515181977));
#26031=CARTESIAN_POINT('Ctrl Pts',(0.651848433300679,0.0875078611215212,
2.52504830080363));
#26032=CARTESIAN_POINT('Ctrl Pts',(0.655499778670142,0.0304708707095967,
2.5535614497875));
#26033=CARTESIAN_POINT('Ctrl Pts',(0.659151124039606,-0.0418338865539044,
2.55153335075717));
#26034=CARTESIAN_POINT('Ctrl Pts',(0.662802469409069,-0.0971828214413289,
2.51986774421674));
#26035=CARTESIAN_POINT('Ctrl Pts',(0.666453814778532,-0.152531756328753,
2.48820213767631));
#26036=CARTESIAN_POINT('Ctrl Pts',(0.670105160147996,-0.190924868840101,
2.42689902362578));
#26037=CARTESIAN_POINT('Ctrl Pts',(0.673756505517459,-0.195251673282228,
2.36327908072691));
#26038=CARTESIAN_POINT('Ctrl Pts',(0.677407850886922,-0.199578477724354,
2.29965913782805));
#26039=CARTESIAN_POINT('Ctrl Pts',(0.681059196256386,-0.16983897409726,
2.23372236608085));
#26040=CARTESIAN_POINT('Ctrl Pts',(0.684710541625849,-0.119287023000938,
2.19485441601494));
#26041=CARTESIAN_POINT('Ctrl Pts',(0.687144704679758,-0.0855866525317966,
2.16894316455599));
#26042=CARTESIAN_POINT('Ctrl Pts',(0.689578867733667,-0.0426368160594284,
2.15506183635612));
#26043=CARTESIAN_POINT('Ctrl Pts',(0.692013030787577,0.000139690484509278,
2.15476836676823));
#26044=CARTESIAN_POINT('Ctrl Pts',(0.702186969212423,0.000153231897286442,
2.15472339864344));
#26045=CARTESIAN_POINT('Ctrl Pts',(0.699646393382886,-0.0444672130138438,
2.15506518181601));
#26046=CARTESIAN_POINT('Ctrl Pts',(0.697105817553348,-0.0892987348503382,
2.17029516368888));
#26047=CARTESIAN_POINT('Ctrl Pts',(0.694565241723811,-0.123683081253107,
2.19833580937399));
#26048=CARTESIAN_POINT('Ctrl Pts',(0.690913896354348,-0.173100667046107,
2.23863615411818));
#26049=CARTESIAN_POINT('Ctrl Pts',(0.687262550984885,-0.200938801892689,
2.30539791832267));
#26050=CARTESIAN_POINT('Ctrl Pts',(0.683611205615422,-0.194791014914288,
2.36886775727776));
#26051=CARTESIAN_POINT('Ctrl Pts',(0.679959860245959,-0.188643227935887,
2.43233759623284));
#26052=CARTESIAN_POINT('Ctrl Pts',(0.676308514876495,-0.148509519132504,
2.49251550993851));
#26053=CARTESIAN_POINT('Ctrl Pts',(0.672657169507032,-0.0922760620207351,
2.52258232978025));
#26054=CARTESIAN_POINT('Ctrl Pts',(0.669005824137568,-0.0360426049089654,
2.55264914962198));
#26055=CARTESIAN_POINT('Ctrl Pts',(0.665354478768105,0.0362906005111901,
2.55260487559978));
#26056=CARTESIAN_POINT('Ctrl Pts',(0.661703133398642,0.0924872190443799,
2.52246925511011));
#26057=CARTESIAN_POINT('Ctrl Pts',(0.658051788029179,0.148683837577569,
2.49233363462045));
#26058=CARTESIAN_POINT('Ctrl Pts',(0.654400442659716,0.188743869223793,
2.43210666766332));
#26059=CARTESIAN_POINT('Ctrl Pts',(0.650749097290252,0.19481396515396,2.36862934437913));
#26060=CARTESIAN_POINT('Ctrl Pts',(0.647097751920789,0.200884061084127,
2.30515202109494));
#26061=CARTESIAN_POINT('Ctrl Pts',(0.643446406551326,0.172964221298237,
2.23842434148368));
#26062=CARTESIAN_POINT('Ctrl Pts',(0.639795061181862,0.123497355969801,
2.19818452650765));
#26063=CARTESIAN_POINT('Ctrl Pts',(0.637259030525382,0.089140297335463,
2.17023608721628));
#26064=CARTESIAN_POINT('Ctrl Pts',(0.634722999868903,0.0443890523714131,
2.15506527237943));
#26065=CARTESIAN_POINT('Ctrl Pts',(0.632186969212423,-0.000152729840347416,
2.15472545757722));
#26066=CARTESIAN_POINT('Origin',(0.7225,0.,2.35));
#26067=CARTESIAN_POINT('',(0.552013030787577,0.000119548669269599,2.15439909884273));
#26068=CARTESIAN_POINT('',(0.562186969212423,8.98932785041182E-5,2.15435395233057));
#26069=CARTESIAN_POINT('',(0.7225,-2.39295984553393E-17,2.1546));
#26070=CARTESIAN_POINT('Ctrl Pts',(0.552013030787577,0.000119548669269599,
2.15439909884273));
#26071=CARTESIAN_POINT('Ctrl Pts',(0.552429389966775,0.00740179500524078,
2.1543504652939));
#26072=CARTESIAN_POINT('Ctrl Pts',(0.552845749145972,0.0146785211588285,
2.1547249528878));
#26073=CARTESIAN_POINT('Ctrl Pts',(0.55326210832517,0.0219052057459278,
2.15554007694822));
#26074=CARTESIAN_POINT('Ctrl Pts',(0.556913453694633,0.0852810663538896,
2.16268847096059));
#26075=CARTESIAN_POINT('Ctrl Pts',(0.560564799064096,0.144808347695821,
2.2037251799862));
#26076=CARTESIAN_POINT('Ctrl Pts',(0.564216144433559,0.173992070839574,
2.26041257816284));
#26077=CARTESIAN_POINT('Ctrl Pts',(0.567867489803023,0.203175793983327,
2.31709997633948));
#26078=CARTESIAN_POINT('Ctrl Pts',(0.571518835172486,0.202015958928901,
2.38943806366715));
#26079=CARTESIAN_POINT('Ctrl Pts',(0.575170180541949,0.171012158196446,
2.44516263247295));
#26080=CARTESIAN_POINT('Ctrl Pts',(0.578821525911413,0.140008357463991,
2.50088720127875));
#26081=CARTESIAN_POINT('Ctrl Pts',(0.582472871280876,0.0791605910535053,
2.53999825156269));
#26082=CARTESIAN_POINT('Ctrl Pts',(0.58612421665034,0.0155953124083451,
2.54507837792627));
#26083=CARTESIAN_POINT('Ctrl Pts',(0.589775562019803,-0.0479699662368153,
2.55015850428984));
#26084=CARTESIAN_POINT('Ctrl Pts',(0.593426907389266,-0.11425275711665,
2.52120770673306));
#26085=CARTESIAN_POINT('Ctrl Pts',(0.597078252758729,-0.153717611658953,
2.47112174316925));
#26086=CARTESIAN_POINT('Ctrl Pts',(0.600729598128193,-0.193182466201255,
2.42103577960544));
#26087=CARTESIAN_POINT('Ctrl Pts',(0.604380943497656,-0.205829384406025,
2.34981465003461));
#26088=CARTESIAN_POINT('Ctrl Pts',(0.608032288867119,-0.186019835097296,
2.28920241992824));
#26089=CARTESIAN_POINT('Ctrl Pts',(0.611683634236583,-0.166210285788567,
2.22859018982187));
#26090=CARTESIAN_POINT('Ctrl Pts',(0.615334979606046,-0.113944268966339,
2.17858685917995));
#26091=CARTESIAN_POINT('Ctrl Pts',(0.618986324975509,-0.0525160324459869,
2.1614754481794));
#26092=CARTESIAN_POINT('Ctrl Pts',(0.619995226912865,-0.0355428183118095,
2.15674740030595));
#26093=CARTESIAN_POINT('Ctrl Pts',(0.621004128850221,-0.0178700960153893,
2.15453055244942));
#26094=CARTESIAN_POINT('Ctrl Pts',(0.622013030787577,-0.000161508074393329,
2.15467656254574));
#26095=CARTESIAN_POINT('Ctrl Pts',(0.632186969212423,-0.000152729840347416,
2.15472545757722));
#26096=CARTESIAN_POINT('Ctrl Pts',(0.631071654499439,-0.0197416511794313,
2.15457601125739));
#26097=CARTESIAN_POINT('Ctrl Pts',(0.629956339786456,-0.039290059680257,
2.157295074489));
#26098=CARTESIAN_POINT('Ctrl Pts',(0.628841025073472,-0.0578960018528886,
2.16305730877361));
#26099=CARTESIAN_POINT('Ctrl Pts',(0.625189679704009,-0.118808603476159,
2.1819218563564));
#26100=CARTESIAN_POINT('Ctrl Pts',(0.621538334334546,-0.169619915851716,
2.23340290186278));
#26101=CARTESIAN_POINT('Ctrl Pts',(0.617886988965082,-0.187685029649559,
2.29455741289086));
#26102=CARTESIAN_POINT('Ctrl Pts',(0.614235643595619,-0.205750143447401,
2.35571192391893));
#26103=CARTESIAN_POINT('Ctrl Pts',(0.610584298226155,-0.191069058667529,
2.42653990046871));
#26104=CARTESIAN_POINT('Ctrl Pts',(0.606932952856692,-0.15018483214835,
2.47547534853885));
#26105=CARTESIAN_POINT('Ctrl Pts',(0.603281607487229,-0.10930060562917,
2.524410796609));
#26106=CARTESIAN_POINT('Ctrl Pts',(0.599630262117766,-0.0422132373706839,
2.55145371619953));
#26107=CARTESIAN_POINT('Ctrl Pts',(0.595978916748303,0.0211792443787588,
2.54455298193631));
#26108=CARTESIAN_POINT('Ctrl Pts',(0.59232757137884,0.0845717261282007,
2.53765224767309));
#26109=CARTESIAN_POINT('Ctrl Pts',(0.588676226009376,0.144269321368599,
2.49680785955613));
#26110=CARTESIAN_POINT('Ctrl Pts',(0.585024880639913,0.173666080429868,
2.44022084897972));
#26111=CARTESIAN_POINT('Ctrl Pts',(0.581373535270449,0.203062839491137,
2.38363383840331));
#26112=CARTESIAN_POINT('Ctrl Pts',(0.577722189900986,0.202158762373277,
2.31130420536744));
#26113=CARTESIAN_POINT('Ctrl Pts',(0.574070844531523,0.171358441495245,
2.25547037582024));
#26114=CARTESIAN_POINT('Ctrl Pts',(0.57041949916206,0.140558120617212,2.19963654627303));
#26115=CARTESIAN_POINT('Ctrl Pts',(0.566768153792596,0.0798615559790066,
2.16029852021448));
#26116=CARTESIAN_POINT('Ctrl Pts',(0.563116808423133,0.0163157428736723,
2.1549806077331));
#26117=CARTESIAN_POINT('Ctrl Pts',(0.562806862019563,0.0109216225588305,
2.15452919388934));
#26118=CARTESIAN_POINT('Ctrl Pts',(0.562496915615993,0.00550697183036078,
2.15432291381032));
#26119=CARTESIAN_POINT('Ctrl Pts',(0.562186969212423,8.98932785041182E-5,
2.15435395233057));
#26120=CARTESIAN_POINT('Origin',(1.05400562256037,0.,2.35));
#26121=CARTESIAN_POINT('',(0.52900562256037,9.51678377910506E-5,2.19429007075223));
#26122=CARTESIAN_POINT('',(0.5204,-2.14950933638427E-15,2.19445));
#26123=CARTESIAN_POINT('',(1.05400562256037,-2.14950933638427E-15,2.19445));
#26124=CARTESIAN_POINT('',(0.5204,-0.108754917490551,2.23849675560759));
#26125=CARTESIAN_POINT('Ctrl Pts',(0.52900562256037,9.51678377910398E-5,
2.19429007075223));
#26126=CARTESIAN_POINT('Ctrl Pts',(0.526137081706913,-0.0398444327547342,
2.19455680225596));
#26127=CARTESIAN_POINT('Ctrl Pts',(0.523268540853457,-0.0799926191159976,
2.21081160130798));
#26128=CARTESIAN_POINT('Ctrl Pts',(0.5204,-0.108759141326515,2.23849470445504));
#26129=CARTESIAN_POINT('Origin',(0.5204,0.,2.35));
#26130=CARTESIAN_POINT('Origin',(1.05400562256037,0.,2.35));
#26131=CARTESIAN_POINT('',(0.59900562256037,-0.000128570015209672,2.19451094833158));
#26132=CARTESIAN_POINT('',(0.58519437743963,7.15603862352279E-5,2.19425413144842));
#26133=CARTESIAN_POINT('',(1.05400562256037,-2.14950933638427E-15,2.19445));
#26134=CARTESIAN_POINT('Ctrl Pts',(0.59900562256037,-0.000128570015209668,
2.19451094833158));
#26135=CARTESIAN_POINT('Ctrl Pts',(0.597996720623014,-0.0142256572937251,
2.19439471562695));
#26136=CARTESIAN_POINT('Ctrl Pts',(0.593336473316195,-0.0792100279504878,
2.20254628731932));
#26137=CARTESIAN_POINT('Ctrl Pts',(0.585024880639913,-0.173920106812228,
2.29315620321465));
#26138=CARTESIAN_POINT('Ctrl Pts',(0.574070844531523,-0.143717013770999,
2.46324494484324));
#26139=CARTESIAN_POINT('Ctrl Pts',(0.563116808423133,0.014578095564083,
2.53238460543625));
#26140=CARTESIAN_POINT('Ctrl Pts',(0.552162772314743,0.159893398509083,
2.43898045182826));
#26141=CARTESIAN_POINT('Ctrl Pts',(0.541208736206353,0.162663291181281,
2.2662242161504));
#26142=CARTESIAN_POINT('Ctrl Pts',(0.533489686288229,0.0624852719175517,
2.19716384358485));
#26143=CARTESIAN_POINT('Ctrl Pts',(0.529421981739568,0.00589226823472279,
2.19425135556021));
#26144=CARTESIAN_POINT('Ctrl Pts',(0.52900562256037,9.51678377910398E-5,
2.19429007075223));
#26145=CARTESIAN_POINT('',(0.5204,0.0700655924093113,2.21112374119263));
#26146=CARTESIAN_POINT('Origin',(0.5204,0.,2.35));
#26147=CARTESIAN_POINT('Ctrl Pts',(0.58519437743963,7.15603862352183E-5,
2.19425413144842));
#26148=CARTESIAN_POINT('Ctrl Pts',(0.581852978473736,-0.046417666264194,
2.19452050321855));
#26149=CARTESIAN_POINT('Ctrl Pts',(0.574860234138379,-0.144178508701954,
2.24102737311269));
#26150=CARTESIAN_POINT('Ctrl Pts',(0.56421614443356,-0.174115819489472,
2.40622641443997));
#26151=CARTESIAN_POINT('Ctrl Pts',(0.55326210832517,-0.0497712388056558,
2.52603005943954));
#26152=CARTESIAN_POINT('Ctrl Pts',(0.54230807221678,0.119016533293403,2.48911101549988));
#26153=CARTESIAN_POINT('Ctrl Pts',(0.53135403610839,0.181561589671221,2.32783318660189));
#26154=CARTESIAN_POINT('Ctrl Pts',(0.524051345369463,0.115581452136368,
2.23408731828768));
#26155=CARTESIAN_POINT('Ctrl Pts',(0.5204,0.0700655924093113,2.21112374119263));
#26156=CARTESIAN_POINT('Origin',(1.05400562256037,0.,2.35));
#26157=CARTESIAN_POINT('',(0.66900562256037,0.000111201918452189,2.19458402994267));
#26158=CARTESIAN_POINT('',(0.655194377439629,-0.000121582019789068,2.19454987167931));
#26159=CARTESIAN_POINT('',(1.05400562256037,-2.14950933638427E-15,2.19445));
#26160=CARTESIAN_POINT('Ctrl Pts',(0.66900562256037,0.0001112019184522,
2.19458402994267));
#26161=CARTESIAN_POINT('Ctrl Pts',(0.666571459506461,-0.0339414367351281,
2.19481764915658));
#26162=CARTESIAN_POINT('Ctrl Pts',(0.660485951083088,-0.11941940134295,
2.22244401000061));
#26163=CARTESIAN_POINT('Ctrl Pts',(0.650749097290252,-0.182550726710429,
2.36241526987937));
#26164=CARTESIAN_POINT('Ctrl Pts',(0.639795061181862,-0.0908611363653908,
2.5088180240845));
#26165=CARTESIAN_POINT('Ctrl Pts',(0.628841025073472,0.0818155011832931,
2.51366148576568));
#26166=CARTESIAN_POINT('Ctrl Pts',(0.617886988965083,0.181567845985935,
2.37262906836985));
#26167=CARTESIAN_POINT('Ctrl Pts',(0.607941854794048,0.125201242106021,
2.22627332924704));
#26168=CARTESIAN_POINT('Ctrl Pts',(0.601648065992477,0.0367935076532955,
2.19481537667645));
#26169=CARTESIAN_POINT('Ctrl Pts',(0.59900562256037,-0.000128570015209668,
2.19451094833158));
#26170=CARTESIAN_POINT('Ctrl Pts',(0.655194377439629,-0.000121582019789061,
2.19454987167931));
#26171=CARTESIAN_POINT('Ctrl Pts',(0.654079062726646,-0.0157155263099339,
2.19443090353678));
#26172=CARTESIAN_POINT('Ctrl Pts',(0.649312402644199,-0.082223484242051,
2.20368175088914));
#26173=CARTESIAN_POINT('Ctrl Pts',(0.640894397192289,-0.175476343657893,
2.29816375646506));
#26174=CARTESIAN_POINT('Ctrl Pts',(0.629940361083899,-0.140415298557959,
2.46731357866031));
#26175=CARTESIAN_POINT('Ctrl Pts',(0.618986324975509,0.0198012848495282,
2.53189688688404));
#26176=CARTESIAN_POINT('Ctrl Pts',(0.60803228886712,0.16236977419923,2.4343532138299));
#26177=CARTESIAN_POINT('Ctrl Pts',(0.597078252758729,0.160210677029069,
2.26161716850653));
#26178=CARTESIAN_POINT('Ctrl Pts',(0.589465615616233,0.0594730344796908,
2.19632813557188));
#26179=CARTESIAN_POINT('Ctrl Pts',(0.5855043238432,0.00438387650057295,
2.19422942294368));
#26180=CARTESIAN_POINT('Ctrl Pts',(0.58519437743963,7.15603862352183E-5,
2.19425413144842));
#26181=CARTESIAN_POINT('Origin',(1.05400562256037,0.,2.35));
#26182=CARTESIAN_POINT('',(0.73900562256037,-4.93584221261508E-5,2.19422991105133));
#26183=CARTESIAN_POINT('',(0.725194377439629,0.000121981686909765,2.19454823264579));
#26184=CARTESIAN_POINT('',(1.05400562256037,-2.14950933638427E-15,2.19445));
#26185=CARTESIAN_POINT('Ctrl Pts',(0.73900562256037,-4.93584221261476E-5,
2.19422991105133));
#26186=CARTESIAN_POINT('Ctrl Pts',(0.738797543759371,-0.00294318160930773,
2.19421764985331));
#26187=CARTESIAN_POINT('Ctrl Pts',(0.734938119588908,-0.0566056877646526,
2.19558775087244));
#26188=CARTESIAN_POINT('Ctrl Pts',(0.727427350048981,-0.157727895671703,
2.2572594409398));
#26189=CARTESIAN_POINT('Ctrl Pts',(0.716473313940592,-0.164621520822112,
2.42986649077344));
#26190=CARTESIAN_POINT('Ctrl Pts',(0.705519277832201,-0.0247832025340387,
2.53128622214169));
#26191=CARTESIAN_POINT('Ctrl Pts',(0.694565241723812,0.137145099584703,
2.47112027917621));
#26192=CARTESIAN_POINT('Ctrl Pts',(0.683611205615422,0.176831999341087,
2.30299632262599));
#26193=CARTESIAN_POINT('Ctrl Pts',(0.675091332560941,0.0851090304351673,
2.20481803865857));
#26194=CARTESIAN_POINT('Ctrl Pts',(0.670222804875924,0.0171389312238162,
2.19446721066252));
#26195=CARTESIAN_POINT('Ctrl Pts',(0.66900562256037,0.0001112019184522,
2.19458402994267));
#26196=CARTESIAN_POINT('Ctrl Pts',(0.725194377439629,0.000121981686909774,
2.19454823264579));
#26197=CARTESIAN_POINT('Ctrl Pts',(0.722653801610092,-0.035398541373101,
2.19482031234125));
#26198=CARTESIAN_POINT('Ctrl Pts',(0.716461880411091,-0.122379100748218,
2.22436899345466));
#26199=CARTESIAN_POINT('Ctrl Pts',(0.706618613842629,-0.182120023079803,
2.36764042281014));
#26200=CARTESIAN_POINT('Ctrl Pts',(0.695664577734238,-0.086273578795776,
2.51135599819781));
#26201=CARTESIAN_POINT('Ctrl Pts',(0.684710541625849,0.0864709980175075,
2.51125026394776));
#26202=CARTESIAN_POINT('Ctrl Pts',(0.673756505517459,0.182141488128614,
2.36741754065941));
#26203=CARTESIAN_POINT('Ctrl Pts',(0.663917784122053,0.122252892767114,
2.22428537964787));
#26204=CARTESIAN_POINT('Ctrl Pts',(0.657730408096109,0.0353363208616827,
2.19482038443511));
#26205=CARTESIAN_POINT('Ctrl Pts',(0.655194377439629,-0.000121582019789061,
2.19454987167931));
#26206=CARTESIAN_POINT('Origin',(1.05400562256037,0.,2.35));
#26207=CARTESIAN_POINT('',(0.80900562256037,-4.08630748678726E-5,2.19467648483088));
#26208=CARTESIAN_POINT('',(0.79519437743963,-7.19606880817819E-5,2.19425418850934));
#26209=CARTESIAN_POINT('',(1.05400562256037,-2.14950933638427E-15,2.19445));
#26210=CARTESIAN_POINT('Ctrl Pts',(0.80900562256037,-4.08630748678709E-5,
2.19467648483088));
#26211=CARTESIAN_POINT('Ctrl Pts',(0.807372282642817,-0.02292474521305,
2.19462097806632));
#26212=CARTESIAN_POINT('Ctrl Pts',(0.802087597355801,-0.0968949254760526,
2.20997973041345));
#26213=CARTESIAN_POINT('Ctrl Pts',(0.793151566699321,-0.180979052586637,
2.32306599395291));
#26214=CARTESIAN_POINT('Ctrl Pts',(0.782197530590931,-0.12274025290824,
2.48569724091423));
#26215=CARTESIAN_POINT('Ctrl Pts',(0.771243494482541,0.0449007034323279,
2.52737765806314));
#26216=CARTESIAN_POINT('Ctrl Pts',(0.760289458374152,0.172520254747402,
2.41095619106118));
#26217=CARTESIAN_POINT('Ctrl Pts',(0.74954350106676,0.146864336702308,2.24344628678707));
#26218=CARTESIAN_POINT('Ctrl Pts',(0.742448889128834,0.0478373296383567,
2.19443280809342));
#26219=CARTESIAN_POINT('Ctrl Pts',(0.73900562256037,-4.93584221261476E-5,
2.19422991105133));
#26220=CARTESIAN_POINT('Ctrl Pts',(0.79519437743963,-7.19606880817871E-5,
2.19425418850934));
#26221=CARTESIAN_POINT('Ctrl Pts',(0.794879885863002,-0.00444751424563119,
2.19422865519439));
#26222=CARTESIAN_POINT('Ctrl Pts',(0.790914048916912,-0.0595994116820262,
2.19635851179074));
#26223=CARTESIAN_POINT('Ctrl Pts',(0.783296866601358,-0.160320194189603,
2.26181657493399));
#26224=CARTESIAN_POINT('Ctrl Pts',(0.772342830492968,-0.16226566916103,
2.43455022864764));
#26225=CARTESIAN_POINT('Ctrl Pts',(0.761388794384578,-0.0195790184948705,
2.53192182210578));
#26226=CARTESIAN_POINT('Ctrl Pts',(0.750434758276188,0.140558966382812,
2.46714120953931));
#26227=CARTESIAN_POINT('Ctrl Pts',(0.739480722167798,0.175412672397597,
2.29794924135903));
#26228=CARTESIAN_POINT('Ctrl Pts',(0.731067261888946,0.0820947684486603,
2.20363214347216));
#26229=CARTESIAN_POINT('Ctrl Pts',(0.726305146979556,0.0156519708329137,
2.19442927621291));
#26230=CARTESIAN_POINT('Ctrl Pts',(0.725194377439629,0.000121981686909774,
2.19454823264579));
#26231=CARTESIAN_POINT('Origin',(1.05400562256037,0.,2.35));
#26232=CARTESIAN_POINT('',(0.87900562256037,0.000124190176919192,2.19434837072514));
#26233=CARTESIAN_POINT('',(0.865194377439629,-1.79285551041297E-5,2.1946855147081));
#26234=CARTESIAN_POINT('',(1.05400562256037,-2.14950933638427E-15,2.19445));
#26235=CARTESIAN_POINT('Ctrl Pts',(0.87900562256037,0.000124190176919186,
2.19434837072514));
#26236=CARTESIAN_POINT('Ctrl Pts',(0.875947021526264,-0.0424956765806325,
2.19470411582899));
#26237=CARTESIAN_POINT('Ctrl Pts',(0.869237075122694,-0.136605475911018,
2.23469767016882));
#26238=CARTESIAN_POINT('Ctrl Pts',(0.858875783349661,-0.177891546494684,
2.39279325713406));
#26239=CARTESIAN_POINT('Ctrl Pts',(0.847921747241271,-0.0630038111484079,
2.52178334424669));
#26240=CARTESIAN_POINT('Ctrl Pts',(0.83696771113288,0.108053315947243,2.49766144283244));
#26241=CARTESIAN_POINT('Ctrl Pts',(0.826013675024491,0.18279317314933,2.34192284359958));
#26242=CARTESIAN_POINT('Ctrl Pts',(0.816692978833654,0.107756578718704,
2.21553286752609));
#26243=CARTESIAN_POINT('Ctrl Pts',(0.81102362801228,0.028232369226284,2.19474506391372));
#26244=CARTESIAN_POINT('Ctrl Pts',(0.80900562256037,-4.08630748678709E-5,
2.19467648483088));
#26245=CARTESIAN_POINT('Ctrl Pts',(0.865194377439629,-1.79285551041419E-5,
2.19468551470809));
#26246=CARTESIAN_POINT('Ctrl Pts',(0.863454624746448,-0.0243964419532612,
2.19465869077632));
#26247=CARTESIAN_POINT('Ctrl Pts',(0.858063526683804,-0.0999055619129348,
2.21143804034893));
#26248=CARTESIAN_POINT('Ctrl Pts',(0.849021083251698,-0.181675685171884,
2.32826261843907));
#26249=CARTESIAN_POINT('Ctrl Pts',(0.838067047143307,-0.118802362076862,
2.48915793391742));
#26250=CARTESIAN_POINT('Ctrl Pts',(0.827113011034918,0.0499644633958529,
2.52601845279664));
#26251=CARTESIAN_POINT('Ctrl Pts',(0.816158974926527,0.174195747659866,
2.40598825754555));
#26252=CARTESIAN_POINT('Ctrl Pts',(0.805519430394765,0.14405268557978,2.24093310845852));
#26253=CARTESIAN_POINT('Ctrl Pts',(0.798531231232466,0.0463540283347385,
2.19452510495093));
#26254=CARTESIAN_POINT('Ctrl Pts',(0.79519437743963,-7.19606880817871E-5,
2.19425418850934));
#26255=CARTESIAN_POINT('Origin',(0.5204,-2.59090492670967E-17,2.35));
#26256=CARTESIAN_POINT('',(0.5204,-0.0584934195161147,2.53643948045763));
#26257=CARTESIAN_POINT('Ctrl Pts',(0.5204,-0.108759141326515,2.23849470445504));
#26258=CARTESIAN_POINT('Ctrl Pts',(0.5204,-0.112907330059273,2.24159827661415));
#26259=CARTESIAN_POINT('Ctrl Pts',(0.5204,-0.116881232068949,2.24491115539772));
#26260=CARTESIAN_POINT('Ctrl Pts',(0.5204,-0.120661377643655,2.24842558763538));
#26261=CARTESIAN_POINT('Ctrl Pts',(0.5204,-0.125564505420802,2.2529840656053));
#26262=CARTESIAN_POINT('Ctrl Pts',(0.5204,-0.130141932979661,2.25788137180214));
#26263=CARTESIAN_POINT('Ctrl Pts',(0.5204,-0.134389577775584,2.26307215460619));
#26264=CARTESIAN_POINT('Ctrl Pts',(0.5204,-0.137535387529399,2.26691645326096));
#26265=CARTESIAN_POINT('Ctrl Pts',(0.5204,-0.140500968847107,2.27092391847997));
#26266=CARTESIAN_POINT('Ctrl Pts',(0.5204,-0.143271491547599,2.27505836426546));
#26267=CARTESIAN_POINT('Ctrl Pts',(0.5204,-0.148395262305637,2.28270455767603));
#26268=CARTESIAN_POINT('Ctrl Pts',(0.5204,-0.15286388444708,2.29079619664306));
#26269=CARTESIAN_POINT('Ctrl Pts',(0.5204,-0.156663462872097,2.29922509487536));
#26270=CARTESIAN_POINT('Ctrl Pts',(0.5204,-0.158675814066677,2.30368924892863));
#26271=CARTESIAN_POINT('Ctrl Pts',(0.5204,-0.160500911014214,2.30825162957441));
#26272=CARTESIAN_POINT('Ctrl Pts',(0.5204,-0.162127268087927,2.31287264211295));
#26273=CARTESIAN_POINT('Ctrl Pts',(0.5204,-0.166006645959223,2.32389522385391));
#26274=CARTESIAN_POINT('Ctrl Pts',(0.5204,-0.168771336018711,2.33527453234392));
#26275=CARTESIAN_POINT('Ctrl Pts',(0.5204,-0.170389890260227,2.34680888322882));
#26276=CARTESIAN_POINT('Ctrl Pts',(0.5204,-0.171128381708844,2.35207161664569));
#26277=CARTESIAN_POINT('Ctrl Pts',(0.5204,-0.171627714504877,2.35736710228387));
#26278=CARTESIAN_POINT('Ctrl Pts',(0.5204,-0.171881743379811,2.36267782474742));
#26279=CARTESIAN_POINT('Ctrl Pts',(0.5204,-0.172104849855246,2.36734208415953));
#26280=CARTESIAN_POINT('Ctrl Pts',(0.5204,-0.172138134548399,2.37202236286416));
#26281=CARTESIAN_POINT('Ctrl Pts',(0.5204,-0.17197823645371,2.37667856889389));
#26282=CARTESIAN_POINT('Ctrl Pts',(0.5204,-0.171715082631453,2.38434156460574));
#26283=CARTESIAN_POINT('Ctrl Pts',(0.5204,-0.170930692380004,2.39195277755355));
#26284=CARTESIAN_POINT('Ctrl Pts',(0.5204,-0.169614423041612,2.39945925007218));
#26285=CARTESIAN_POINT('Ctrl Pts',(0.5204,-0.168268512776876,2.40713476003059));
#26286=CARTESIAN_POINT('Ctrl Pts',(0.5204,-0.166366695988795,2.41470100550351));
#26287=CARTESIAN_POINT('Ctrl Pts',(0.5204,-0.163950619192884,2.42212362412655));
#26288=CARTESIAN_POINT('Ctrl Pts',(0.5204,-0.162575528939075,2.42634814651903));
#26289=CARTESIAN_POINT('Ctrl Pts',(0.5204,-0.161033657153843,2.43052615011737));
#26290=CARTESIAN_POINT('Ctrl Pts',(0.5204,-0.159331206362488,2.43465111681409));
#26291=CARTESIAN_POINT('Ctrl Pts',(0.5204,-0.157858857773026,2.43821855554908));
#26292=CARTESIAN_POINT('Ctrl Pts',(0.5204,-0.156269236378672,2.44173904368652));
#26293=CARTESIAN_POINT('Ctrl Pts',(0.5204,-0.154570626304257,2.44520268317124));
#26294=CARTESIAN_POINT('Ctrl Pts',(0.5204,-0.149623492625337,2.45529039417953));
#26295=CARTESIAN_POINT('Ctrl Pts',(0.5204,-0.143748121077635,2.46491226866532));
#26296=CARTESIAN_POINT('Ctrl Pts',(0.5204,-0.137061858098255,2.47397051071086));
#26297=CARTESIAN_POINT('Ctrl Pts',(0.5204,-0.132163446938004,2.48060665321153));
#26298=CARTESIAN_POINT('Ctrl Pts',(0.5204,-0.126828911752323,2.48694038241048));
#26299=CARTESIAN_POINT('Ctrl Pts',(0.5204,-0.121092850543412,2.49292921348278));
#26300=CARTESIAN_POINT('Ctrl Pts',(0.5204,-0.118821952815951,2.49530018240674));
#26301=CARTESIAN_POINT('Ctrl Pts',(0.5204,-0.116489100525108,2.49761568017534));
#26302=CARTESIAN_POINT('Ctrl Pts',(0.5204,-0.114103581939124,2.49986675461349));
#26303=CARTESIAN_POINT('Ctrl Pts',(0.5204,-0.10477538102635,2.5086692325116));
#26304=CARTESIAN_POINT('Ctrl Pts',(0.5204,-0.0946182126828188,2.51651747522707));
#26305=CARTESIAN_POINT('Ctrl Pts',(0.5204,-0.0837748677305257,2.52326941089188));
#26306=CARTESIAN_POINT('Ctrl Pts',(0.5204,-0.0757132037363705,2.52828924903955));
#26307=CARTESIAN_POINT('Ctrl Pts',(0.5204,-0.0672710749325205,2.53270298831844));
#26308=CARTESIAN_POINT('Ctrl Pts',(0.5204,-0.058493419516116,2.53643948045763));
#26309=CARTESIAN_POINT('',(0.5204,-2.39295984553393E-17,2.1546));
#26310=CARTESIAN_POINT('Origin',(0.5204,0.,2.35));
#26311=CARTESIAN_POINT('',(0.5204,0.112041393629813,2.51041297594259));
#26312=CARTESIAN_POINT('Origin',(0.5204,0.,2.35));
#26313=CARTESIAN_POINT('Ctrl Pts',(0.5204,0.112041393629812,2.51041297594259));
#26314=CARTESIAN_POINT('Ctrl Pts',(0.5204,0.116937045114913,2.50627340682946));
#26315=CARTESIAN_POINT('Ctrl Pts',(0.5204,0.121606025691287,2.50188933924213));
#26316=CARTESIAN_POINT('Ctrl Pts',(0.5204,0.1260235014566,2.49726406054717));
#26317=CARTESIAN_POINT('Ctrl Pts',(0.5204,0.132755493122292,2.49021538857244));
#26318=CARTESIAN_POINT('Ctrl Pts',(0.5204,0.138904187281487,2.48260660874921));
#26319=CARTESIAN_POINT('Ctrl Pts',(0.5204,0.144439872512489,2.47452670862429));
#26320=CARTESIAN_POINT('Ctrl Pts',(0.5204,0.146734801839087,2.47117702399107));
#26321=CARTESIAN_POINT('Ctrl Pts',(0.5204,0.148922511137616,2.46774842779565));
#26322=CARTESIAN_POINT('Ctrl Pts',(0.5204,0.150996712083198,2.46425475963724));
#26323=CARTESIAN_POINT('Ctrl Pts',(0.5204,0.154797431035443,2.45785304103288));
#26324=CARTESIAN_POINT('Ctrl Pts',(0.5204,0.158222183852141,2.45122603720417));
#26325=CARTESIAN_POINT('Ctrl Pts',(0.5204,0.161257886649128,2.44441406179352));
#26326=CARTESIAN_POINT('Ctrl Pts',(0.5204,0.163547894840152,2.43927539027964));
#26327=CARTESIAN_POINT('Ctrl Pts',(0.5204,0.165616393075825,2.43403139932254));
#26328=CARTESIAN_POINT('Ctrl Pts',(0.5204,0.167455419852478,2.42869927944118));
#26329=CARTESIAN_POINT('Ctrl Pts',(0.5204,0.1688297887935,2.42471440002139));
#26330=CARTESIAN_POINT('Ctrl Pts',(0.5204,0.1700730662053,2.42068834043065));
#26331=CARTESIAN_POINT('Ctrl Pts',(0.5204,0.171181794352447,2.41663368257067));
#26332=CARTESIAN_POINT('Ctrl Pts',(0.5204,0.174401260833582,2.40485998032791));
#26333=CARTESIAN_POINT('Ctrl Pts',(0.5204,0.176494813205288,2.39283081517787));
#26334=CARTESIAN_POINT('Ctrl Pts',(0.5204,0.177388397835593,2.38072640253141));
#26335=CARTESIAN_POINT('Ctrl Pts',(0.5204,0.177810038893935,2.37501489274734));
#26336=CARTESIAN_POINT('Ctrl Pts',(0.5204,0.177963781655902,2.36928669844613));
#26337=CARTESIAN_POINT('Ctrl Pts',(0.5204,0.177837820477668,2.36356196196988));
#26338=CARTESIAN_POINT('Ctrl Pts',(0.5204,0.177744132474277,2.35930399028433));
#26339=CARTESIAN_POINT('Ctrl Pts',(0.5204,0.177495088766334,2.35504632454376));
#26340=CARTESIAN_POINT('Ctrl Pts',(0.5204,0.177088122483941,2.35081883251768));
#26341=CARTESIAN_POINT('Ctrl Pts',(0.5204,0.176379013755951,2.34345273949499));
#26342=CARTESIAN_POINT('Ctrl Pts',(0.5204,0.175191118127969,2.33616306535315));
#26343=CARTESIAN_POINT('Ctrl Pts',(0.5204,0.173504620809491,2.32899257319754));
#26344=CARTESIAN_POINT('Ctrl Pts',(0.5204,0.17195948112857,2.32242309227399));
#26345=CARTESIAN_POINT('Ctrl Pts',(0.5204,0.169995611849258,2.31595359739138));
#26346=CARTESIAN_POINT('Ctrl Pts',(0.5204,0.167635724455005,2.30961315508381));
#26347=CARTESIAN_POINT('Ctrl Pts',(0.5204,0.165837815689064,2.30478261239246));
#26348=CARTESIAN_POINT('Ctrl Pts',(0.5204,0.163809931535238,2.3000270249417));
#26349=CARTESIAN_POINT('Ctrl Pts',(0.5204,0.161560656715894,2.29536084562219));
#26350=CARTESIAN_POINT('Ctrl Pts',(0.5204,0.160071713441668,2.29227199393792));
#26351=CARTESIAN_POINT('Ctrl Pts',(0.5204,0.158487800659087,2.28922696718331));
#26352=CARTESIAN_POINT('Ctrl Pts',(0.5204,0.156815851991927,2.28623595701929));
#26353=CARTESIAN_POINT('Ctrl Pts',(0.5204,0.152047341533174,2.27770539413208));
#26354=CARTESIAN_POINT('Ctrl Pts',(0.5204,0.14655595542121,2.26959575714595));
#26355=CARTESIAN_POINT('Ctrl Pts',(0.5204,0.140413115121167,2.26199694931317));
#26356=CARTESIAN_POINT('Ctrl Pts',(0.5204,0.136686501207848,2.25738705851167));
#26357=CARTESIAN_POINT('Ctrl Pts',(0.5204,0.132719734840018,2.25296552232463));
#26358=CARTESIAN_POINT('Ctrl Pts',(0.5204,0.128526293595978,2.24875666671166));
#26359=CARTESIAN_POINT('Ctrl Pts',(0.5204,0.12615221987615,2.24637386630507));
#26360=CARTESIAN_POINT('Ctrl Pts',(0.5204,0.123703674799012,2.24405772039151));
#26361=CARTESIAN_POINT('Ctrl Pts',(0.5204,0.121188860554935,2.24181840024681));
#26362=CARTESIAN_POINT('Ctrl Pts',(0.5204,0.113088816925757,2.23460570415423));
#26363=CARTESIAN_POINT('Ctrl Pts',(0.5204,0.104340638126238,2.22821818956216));
#26364=CARTESIAN_POINT('Ctrl Pts',(0.5204,0.095037049653237,2.22279264290421));
#26365=CARTESIAN_POINT('Ctrl Pts',(0.5204,0.0871009281534262,2.21816455798781));
#26366=CARTESIAN_POINT('Ctrl Pts',(0.5204,0.0787597846219885,2.2142367405948));
#26367=CARTESIAN_POINT('Ctrl Pts',(0.5204,0.0700655924093113,2.21112374119263));
#26368=CARTESIAN_POINT('Ctrl Pts',(0.947607408227206,0.139614588036676,
2.28141742708713));
#26369=CARTESIAN_POINT('Ctrl Pts',(0.943956062857743,0.117137061674501,
2.23565958438961));
#26370=CARTESIAN_POINT('Ctrl Pts',(0.936653372118816,0.0240992050028806,
2.16868478613642));
#26371=CARTESIAN_POINT('Ctrl Pts',(0.925699336010427,-0.13783558819615,
2.22950867061399));
#26372=CARTESIAN_POINT('Ctrl Pts',(0.914745299902037,-0.17655014467161,
2.39789367865357));
#26373=CARTESIAN_POINT('Ctrl Pts',(0.903791263793647,-0.0580775762076774,
2.52350712786254));
#26374=CARTESIAN_POINT('Ctrl Pts',(0.892837227685257,0.112250391536416,
2.49451043435059));
#26375=CARTESIAN_POINT('Ctrl Pts',(0.881883191576867,0.182481185996413,
2.33668621664117));
#26376=CARTESIAN_POINT('Ctrl Pts',(0.870929155468477,0.09008407841159,2.19073969498444));
#26377=CARTESIAN_POINT('Ctrl Pts',(0.859975119360086,-0.0826191757791262,
2.18674106440834));
#26378=CARTESIAN_POINT('Ctrl Pts',(0.849021083251698,-0.181675685171884,
2.32826261843907));
#26379=CARTESIAN_POINT('Ctrl Pts',(0.838067047143307,-0.118802362076862,
2.48915793391742));
#26380=CARTESIAN_POINT('Ctrl Pts',(0.827113011034918,0.0499644633958529,
2.52601845279664));
#26381=CARTESIAN_POINT('Ctrl Pts',(0.816158974926527,0.174195747659866,
2.40598825754555));
#26382=CARTESIAN_POINT('Ctrl Pts',(0.805204938818138,0.14316169451436,2.23605428550592));
#26383=CARTESIAN_POINT('Ctrl Pts',(0.794250902709748,-0.0154767280957943,
2.16768334330683));
#26384=CARTESIAN_POINT('Ctrl Pts',(0.783296866601358,-0.160320194189603,
2.26181657493399));
#26385=CARTESIAN_POINT('Ctrl Pts',(0.772342830492968,-0.16226566916103,
2.43455022864764));
#26386=CARTESIAN_POINT('Ctrl Pts',(0.761388794384578,-0.0195790184948705,
2.53192182210578));
#26387=CARTESIAN_POINT('Ctrl Pts',(0.750434758276188,0.140558966382812,
2.46714120953931));
#26388=CARTESIAN_POINT('Ctrl Pts',(0.739480722167798,0.175412672397597,
2.29794924135903));
#26389=CARTESIAN_POINT('Ctrl Pts',(0.728526686059409,0.0539159688373249,
2.17515162163435));
#26390=CARTESIAN_POINT('Ctrl Pts',(0.717572649951018,-0.115637599199776,
2.20820143987244));
#26391=CARTESIAN_POINT('Ctrl Pts',(0.706618613842629,-0.182120023079803,
2.36764042281014));
#26392=CARTESIAN_POINT('Ctrl Pts',(0.695664577734238,-0.086273578795776,
2.51135599819781));
#26393=CARTESIAN_POINT('Ctrl Pts',(0.684710541625849,0.0864709980175075,
2.51125026394776));
#26394=CARTESIAN_POINT('Ctrl Pts',(0.673756505517459,0.182141488128614,
2.36741754065941));
#26395=CARTESIAN_POINT('Ctrl Pts',(0.662802469409069,0.115463938302179,
2.20805995780069));
#26396=CARTESIAN_POINT('Ctrl Pts',(0.651848433300678,-0.0541298804027574,
2.17521785121658));
#26397=CARTESIAN_POINT('Ctrl Pts',(0.640894397192289,-0.175476343657893,
2.29816375646506));
#26398=CARTESIAN_POINT('Ctrl Pts',(0.629940361083899,-0.140415298557959,
2.46731357866031));
#26399=CARTESIAN_POINT('Ctrl Pts',(0.618986324975509,0.0198012848495282,
2.53189688688404));
#26400=CARTESIAN_POINT('Ctrl Pts',(0.60803228886712,0.16236977419923,2.4343532138299));
#26401=CARTESIAN_POINT('Ctrl Pts',(0.597078252758729,0.160210677029069,
2.26161716850653));
#26402=CARTESIAN_POINT('Ctrl Pts',(0.58612421665034,0.0152564708447366,
2.16767095632525));
#26403=CARTESIAN_POINT('Ctrl Pts',(0.575170180541949,-0.143306760899327,
2.23621692429532));
#26404=CARTESIAN_POINT('Ctrl Pts',(0.56421614443356,-0.174115819489472,
2.40622641443997));
#26405=CARTESIAN_POINT('Ctrl Pts',(0.55326210832517,-0.0497712388056558,
2.52603005943954));
#26406=CARTESIAN_POINT('Ctrl Pts',(0.54230807221678,0.119016533293403,2.48911101549988));
#26407=CARTESIAN_POINT('Ctrl Pts',(0.53135403610839,0.181561589671221,2.32783318660189));
#26408=CARTESIAN_POINT('Ctrl Pts',(0.524051345369463,0.115581452136368,
2.23408731828768));
#26409=CARTESIAN_POINT('Ctrl Pts',(0.5204,0.0700655924093113,2.21112374119263));
#26410=CARTESIAN_POINT('Ctrl Pts',(0.939938272151471,0.151537102412036,
2.27556075606907));
#26411=CARTESIAN_POINT('Ctrl Pts',(0.936286926782008,0.127140087299121,
2.22589538089218));
#26412=CARTESIAN_POINT('Ctrl Pts',(0.928984236043081,0.0261571784720005,
2.15320120899624));
#26413=CARTESIAN_POINT('Ctrl Pts',(0.918030199934692,-0.14960618326658,
2.21921920425583));
#26414=CARTESIAN_POINT('Ctrl Pts',(0.907076163826301,-0.191626804406237,
2.4019836027816));
#26415=CARTESIAN_POINT('Ctrl Pts',(0.896122127717911,-0.0630371635041008,
2.53832392641675));
#26416=CARTESIAN_POINT('Ctrl Pts',(0.885168091609522,0.121836115532401,
2.50685103396244));
#26417=CARTESIAN_POINT('Ctrl Pts',(0.874214055501131,0.198064332384406,
2.33554927403568));
#26418=CARTESIAN_POINT('Ctrl Pts',(0.863260019392742,0.0977768899935077,
2.17713951678907));
#26419=CARTESIAN_POINT('Ctrl Pts',(0.852305983284352,-0.0896745152301024,
2.17279941952818));
#26420=CARTESIAN_POINT('Ctrl Pts',(0.841351947175961,-0.19719004508638,
2.32640633502494));
#26421=CARTESIAN_POINT('Ctrl Pts',(0.830397911067572,-0.128947597539763,
2.50104145190009));
#26422=CARTESIAN_POINT('Ctrl Pts',(0.819443874959181,0.0542312240651439,
2.54104970822135));
#26423=CARTESIAN_POINT('Ctrl Pts',(0.808489838850793,0.189071351526245,
2.41076942557982));
#26424=CARTESIAN_POINT('Ctrl Pts',(0.797535802742401,0.155387117264596,
2.22632378786831));
#26425=CARTESIAN_POINT('Ctrl Pts',(0.786581766634013,-0.0167983773288753,
2.15211424704791));
#26426=CARTESIAN_POINT('Ctrl Pts',(0.775627730525622,-0.174010882582308,
2.2542860713684));
#26427=CARTESIAN_POINT('Ctrl Pts',(0.764673694417233,-0.176122493153459,
2.44177047210978));
#26428=CARTESIAN_POINT('Ctrl Pts',(0.753719658308842,-0.0212509865373449,
2.54745720110699));
#26429=CARTESIAN_POINT('Ctrl Pts',(0.742765622200452,0.152562126803587,
2.47714458937461));
#26430=CARTESIAN_POINT('Ctrl Pts',(0.731811586092063,0.190392196655701,
2.29350431961502));
#26431=CARTESIAN_POINT('Ctrl Pts',(0.720857549983673,0.0585201718977931,
2.16022028577691));
#26432=CARTESIAN_POINT('Ctrl Pts',(0.709903513875282,-0.125512576866359,
2.19609242321952));
#26433=CARTESIAN_POINT('Ctrl Pts',(0.698949477766893,-0.197672327632959,
2.36914684271581));
#26434=CARTESIAN_POINT('Ctrl Pts',(0.687995441658503,-0.093640989306891,
2.52513514001327));
#26435=CARTESIAN_POINT('Ctrl Pts',(0.677041405550113,0.0938552673221205,
2.52502037649103));
#26436=CARTESIAN_POINT('Ctrl Pts',(0.666087369441724,0.197695625709081,
2.36890492734167));
#26437=CARTESIAN_POINT('Ctrl Pts',(0.655133333333334,0.125324086038902,
2.19593885915794));
#26438=CARTESIAN_POINT('Ctrl Pts',(0.644179297224943,-0.0587523506353723,
2.16029217109439));
#26439=CARTESIAN_POINT('Ctrl Pts',(0.633225261116554,-0.19046130518102,
2.2937371534331));
#26440=CARTESIAN_POINT('Ctrl Pts',(0.622271225008164,-0.152406190334525,
2.47733167811303));
#26441=CARTESIAN_POINT('Ctrl Pts',(0.611317188899773,0.021492233528953,
2.54743013651938));
#26442=CARTESIAN_POINT('Ctrl Pts',(0.600363152791384,0.176235488335819,
2.44155663303299));
#26443=CARTESIAN_POINT('Ctrl Pts',(0.589409116682993,0.173892013104519,
2.25406963644822));
#26444=CARTESIAN_POINT('Ctrl Pts',(0.578455080574605,0.0165593110100914,
2.15210080226881));
#26445=CARTESIAN_POINT('Ctrl Pts',(0.567501044466214,-0.155544571725081,
2.22650031534464));
#26446=CARTESIAN_POINT('Ctrl Pts',(0.556547008357824,-0.188984597817245,
2.41102792009824));
#26447=CARTESIAN_POINT('Ctrl Pts',(0.545592972249434,-0.0540214988858134,
2.54106230602406));
#26448=CARTESIAN_POINT('Ctrl Pts',(0.534638936141044,0.129180058101593,
2.50099052684172));
#26449=CARTESIAN_POINT('Ctrl Pts',(0.523684900032654,0.197066206296954,
2.32594023146654));
#26450=CARTESIAN_POINT('Ctrl Pts',(0.516382209293728,0.125451635073546,
2.22418884970044));
#26451=CARTESIAN_POINT('Ctrl Pts',(0.512730863924265,0.0760489072223641,
2.19926427711147));
#26452=CARTESIAN_POINT('Ctrl Pts',(0.932269136075735,0.163459616787395,
2.26970408505101));
#26453=CARTESIAN_POINT('Ctrl Pts',(0.928617790706272,0.137143112923741,
2.21613117739475));
#26454=CARTESIAN_POINT('Ctrl Pts',(0.921315099967345,0.0282151519411206,
2.13771763185606));
#26455=CARTESIAN_POINT('Ctrl Pts',(0.910361063858956,-0.161376778337011,
2.20892973789767));
#26456=CARTESIAN_POINT('Ctrl Pts',(0.899407027750565,-0.206703464140864,
2.40607352690963));
#26457=CARTESIAN_POINT('Ctrl Pts',(0.888452991642176,-0.0679967508005241,
2.55314072497096));
#26458=CARTESIAN_POINT('Ctrl Pts',(0.877498955533787,0.131421839528385,
2.5191916335743));
#26459=CARTESIAN_POINT('Ctrl Pts',(0.866544919425395,0.213647478772399,
2.3344123314302));
#26460=CARTESIAN_POINT('Ctrl Pts',(0.855590883317007,0.105469701575425,
2.16353933859369));
#26461=CARTESIAN_POINT('Ctrl Pts',(0.844636847208615,-0.0967298546810787,
2.15885777464802));
#26462=CARTESIAN_POINT('Ctrl Pts',(0.833682811100226,-0.212704405000876,
2.32455005161081));
#26463=CARTESIAN_POINT('Ctrl Pts',(0.822728774991836,-0.139092833002665,
2.51292496988275));
#26464=CARTESIAN_POINT('Ctrl Pts',(0.811774738883447,0.0584979847344349,
2.55608096364608));
#26465=CARTESIAN_POINT('Ctrl Pts',(0.800820702775056,0.203946955392624,
2.41555059361408));
#26466=CARTESIAN_POINT('Ctrl Pts',(0.789866666666667,0.167612540014831,
2.2165932902307));
#26467=CARTESIAN_POINT('Ctrl Pts',(0.778912630558277,-0.0181200265619565,
2.13654515078899));
#26468=CARTESIAN_POINT('Ctrl Pts',(0.767958594449887,-0.187701570975013,
2.24675556780282));
#26469=CARTESIAN_POINT('Ctrl Pts',(0.757004558341496,-0.189979317145888,
2.44899071557192));
#26470=CARTESIAN_POINT('Ctrl Pts',(0.746050522233108,-0.0229229545798194,
2.5629925801082));
#26471=CARTESIAN_POINT('Ctrl Pts',(0.735096486124716,0.164565287224363,
2.48714796920991));
#26472=CARTESIAN_POINT('Ctrl Pts',(0.724142450016328,0.205371720913805,
2.28905939787101));
#26473=CARTESIAN_POINT('Ctrl Pts',(0.713188413907937,0.0631243749582614,
2.14528894991948));
#26474=CARTESIAN_POINT('Ctrl Pts',(0.702234377799548,-0.135387554532942,
2.18398340656661));
#26475=CARTESIAN_POINT('Ctrl Pts',(0.691280341691157,-0.213224632186115,
2.37065326262149));
#26476=CARTESIAN_POINT('Ctrl Pts',(0.680326305582768,-0.101008399818006,
2.53891428182873));
#26477=CARTESIAN_POINT('Ctrl Pts',(0.669372269474378,0.101239536626733,
2.53879048903431));
#26478=CARTESIAN_POINT('Ctrl Pts',(0.658418233365987,0.213249763289549,
2.37039231402393));
#26479=CARTESIAN_POINT('Ctrl Pts',(0.647464197257598,0.135184233775625,
2.18381776051518));
#26480=CARTESIAN_POINT('Ctrl Pts',(0.636510161149208,-0.0633748208679874,
2.1453664909722));
#26481=CARTESIAN_POINT('Ctrl Pts',(0.625556125040818,-0.205446266704147,
2.28931055040113));
#26482=CARTESIAN_POINT('Ctrl Pts',(0.614602088932428,-0.164397082111091,
2.48734977756575));
#26483=CARTESIAN_POINT('Ctrl Pts',(0.603648052824038,0.0231831822083779,
2.56296338615472));
#26484=CARTESIAN_POINT('Ctrl Pts',(0.592694016715648,0.190101202472408,
2.44876005223608));
#26485=CARTESIAN_POINT('Ctrl Pts',(0.581739980607259,0.187573349179968,
2.2465221043899));
#26486=CARTESIAN_POINT('Ctrl Pts',(0.570785944498868,0.0178621511754463,
2.13653064821237));
#26487=CARTESIAN_POINT('Ctrl Pts',(0.559831908390479,-0.167782382550835,
2.21678370639397));
#26488=CARTESIAN_POINT('Ctrl Pts',(0.548877872282088,-0.203853376145018,
2.41582942575652));
#26489=CARTESIAN_POINT('Ctrl Pts',(0.537923836173699,-0.0582717589659708,
2.55609455260858));
#26490=CARTESIAN_POINT('Ctrl Pts',(0.526969800065308,0.139343582909784,
2.51287003818356));
#26491=CARTESIAN_POINT('Ctrl Pts',(0.516015763956919,0.212570822922687,
2.32404727633118));
#26492=CARTESIAN_POINT('Ctrl Pts',(0.508713073217992,0.135321818010725,
2.2142903811132));
#26493=CARTESIAN_POINT('Ctrl Pts',(0.505061727848529,0.082032222035417,
2.18740481303031));
#26494=CARTESIAN_POINT('Ctrl Pts',(0.9246,0.175382131162755,2.26384741403295));
#26495=CARTESIAN_POINT('Ctrl Pts',(0.920948654630537,0.147146138548361,
2.20636697389733));
#26496=CARTESIAN_POINT('Ctrl Pts',(0.913645963891609,0.0302731254102407,
2.12223405471588));
#26497=CARTESIAN_POINT('Ctrl Pts',(0.90269192778322,-0.173147373407442,
2.19864027153952));
#26498=CARTESIAN_POINT('Ctrl Pts',(0.89173789167483,-0.221780123875491,
2.41016345103765));
#26499=CARTESIAN_POINT('Ctrl Pts',(0.88078385556644,-0.0729563380969478,
2.56795752352517));
#26500=CARTESIAN_POINT('Ctrl Pts',(0.86982981945805,0.141007563524369,2.53153223318615));
#26501=CARTESIAN_POINT('Ctrl Pts',(0.85887578334966,0.229230625160392,2.33327538882471));
#26502=CARTESIAN_POINT('Ctrl Pts',(0.84792174724127,0.113162513157343,2.14993916039833));
#26503=CARTESIAN_POINT('Ctrl Pts',(0.836967711132881,-0.103785194132055,
2.14491612976786));
#26504=CARTESIAN_POINT('Ctrl Pts',(0.82601367502449,-0.228218764915372,
2.32269376819669));
#26505=CARTESIAN_POINT('Ctrl Pts',(0.815059638916101,-0.149238068465566,
2.52480848786541));
#26506=CARTESIAN_POINT('Ctrl Pts',(0.80410560280771,0.0627647454037258,
2.5711122190708));
#26507=CARTESIAN_POINT('Ctrl Pts',(0.793151566699321,0.218822559259003,
2.42033176164835));
#26508=CARTESIAN_POINT('Ctrl Pts',(0.782197530590931,0.179837962765066,
2.2068627925931));
#26509=CARTESIAN_POINT('Ctrl Pts',(0.771243494482542,-0.0194416757950376,
2.12097605453008));
#26510=CARTESIAN_POINT('Ctrl Pts',(0.760289458374151,-0.201392259367717,
2.23922506423723));
#26511=CARTESIAN_POINT('Ctrl Pts',(0.749335422265762,-0.203836141138318,
2.45621095903406));
#26512=CARTESIAN_POINT('Ctrl Pts',(0.73838138615737,-0.0245949226222939,
2.57852795910941));
#26513=CARTESIAN_POINT('Ctrl Pts',(0.727427350048983,0.176568447645139,
2.49715134904521));
#26514=CARTESIAN_POINT('Ctrl Pts',(0.71647331394059,0.220351245171909,2.284614476127));
#26515=CARTESIAN_POINT('Ctrl Pts',(0.705519277832203,0.0677285780187295,
2.13035761406204));
#26516=CARTESIAN_POINT('Ctrl Pts',(0.69456524172381,-0.145262532199525,
2.17187438991369));
#26517=CARTESIAN_POINT('Ctrl Pts',(0.683611205615423,-0.228776936739271,
2.37215968252717));
#26518=CARTESIAN_POINT('Ctrl Pts',(0.672657169507031,-0.108375810329121,
2.55269342364419));
#26519=CARTESIAN_POINT('Ctrl Pts',(0.661703133398642,0.108623805931346,
2.55256060157758));
#26520=CARTESIAN_POINT('Ctrl Pts',(0.650749097290252,0.228803900870016,
2.3718797007062));
#26521=CARTESIAN_POINT('Ctrl Pts',(0.639795061181862,0.145044381512348,
2.17169666187242));
#26522=CARTESIAN_POINT('Ctrl Pts',(0.628841025073472,-0.0679972911006022,
2.13044081085001));
#26523=CARTESIAN_POINT('Ctrl Pts',(0.617886988965083,-0.220431228227273,
2.28488394736916));
#26524=CARTESIAN_POINT('Ctrl Pts',(0.606932952856692,-0.176387973887657,
2.49736787701848));
#26525=CARTESIAN_POINT('Ctrl Pts',(0.595978916748303,0.0248741308878026,
2.57849663579005));
#26526=CARTESIAN_POINT('Ctrl Pts',(0.585024880639912,0.203966916608997,
2.45596347143917));
#26527=CARTESIAN_POINT('Ctrl Pts',(0.574070844531523,0.201254685255417,
2.23897457233158));
#26528=CARTESIAN_POINT('Ctrl Pts',(0.563116808423133,0.0191649913408013,
2.12096049415593));
#26529=CARTESIAN_POINT('Ctrl Pts',(0.552162772314743,-0.180020193376589,
2.2070670974433));
#26530=CARTESIAN_POINT('Ctrl Pts',(0.541208736206353,-0.218722154472792,
2.42063093141479));
#26531=CARTESIAN_POINT('Ctrl Pts',(0.530254700097963,-0.0625220190461283,
2.5711267991931));
#26532=CARTESIAN_POINT('Ctrl Pts',(0.519300663989573,0.149507107717974,
2.5247495495254));
#26533=CARTESIAN_POINT('Ctrl Pts',(0.508346627881183,0.228075439548419,
2.32215432119582));
#26534=CARTESIAN_POINT('Ctrl Pts',(0.501043937142257,0.145192000947903,
2.20439191252596));
#26535=CARTESIAN_POINT('Ctrl Pts',(0.497392591772793,0.0880155368484699,
2.17554534894914));
#26536=CARTESIAN_POINT('Ctrl Pts',(0.562186969212423,8.98932785041182E-5,
2.15435395233057));
#26537=CARTESIAN_POINT('Ctrl Pts',(0.55884557024653,-0.0583093023980897,
2.15468856527743));
#26538=CARTESIAN_POINT('Ctrl Pts',(0.555504171280636,-0.116990661393897,
2.18260451055754));
#26539=CARTESIAN_POINT('Ctrl Pts',(0.552162772314743,-0.153272989439724,
2.22830996922398));
#26540=CARTESIAN_POINT('Ctrl Pts',(0.54851142694528,-0.192920847075323,
2.27825504210046));
#26541=CARTESIAN_POINT('Ctrl Pts',(0.544860081575816,-0.205821500774057,
2.34944298675763));
#26542=CARTESIAN_POINT('Ctrl Pts',(0.541208736206353,-0.18623847171898,
2.41011960371593));
#26543=CARTESIAN_POINT('Ctrl Pts',(0.53755739083689,-0.166655442663903,
2.47079622067423));
#26544=CARTESIAN_POINT('Ctrl Pts',(0.533906045467426,-0.114588730855015,
2.52096150993366));
#26545=CARTESIAN_POINT('Ctrl Pts',(0.530254700097963,-0.0532171871565546,
2.5383146129521));
#26546=CARTESIAN_POINT('Ctrl Pts',(0.526969800065309,0.00199517034463643,
2.55392617606213));
#26547=CARTESIAN_POINT('Ctrl Pts',(0.523684900032654,0.0647384302451143,
2.54298106678724));
#26548=CARTESIAN_POINT('Ctrl Pts',(0.5204,0.112041393629813,2.51041297594259));
#26549=CARTESIAN_POINT('',(0.9246,-0.126741110252901,2.25945345876159));
#26550=CARTESIAN_POINT('Ctrl Pts',(0.9246,-0.126741110252901,2.25945345876159));
#26551=CARTESIAN_POINT('Ctrl Pts',(0.9246,-0.124304124022258,2.25488172588014));
#26552=CARTESIAN_POINT('Ctrl Pts',(0.9246,-0.121633769967844,2.25045043925615));
#26553=CARTESIAN_POINT('Ctrl Pts',(0.9246,-0.118734751471793,2.2461800207472));
#26554=CARTESIAN_POINT('Ctrl Pts',(0.9246,-0.114974511847176,2.24064097471734));
#26555=CARTESIAN_POINT('Ctrl Pts',(0.9246,-0.110829871551607,2.23537234093936));
#26556=CARTESIAN_POINT('Ctrl Pts',(0.9246,-0.106345035557317,2.23038504832899));
#26557=CARTESIAN_POINT('Ctrl Pts',(0.9246,-0.103023561747274,2.22669145467038));
#26558=CARTESIAN_POINT('Ctrl Pts',(0.9246,-0.099513421358034,2.2231511932741));
#26559=CARTESIAN_POINT('Ctrl Pts',(0.9246,-0.0958481261183665,2.21978442243891));
#26560=CARTESIAN_POINT('Ctrl Pts',(0.9246,-0.0890698117805493,2.21355817611166));
#26561=CARTESIAN_POINT('Ctrl Pts',(0.9246,-0.0817516800897092,2.20791171578257));
#26562=CARTESIAN_POINT('Ctrl Pts',(0.9246,-0.0739985396384171,2.2028752168707));
#26563=CARTESIAN_POINT('Ctrl Pts',(0.9246,-0.0698919378516735,2.20020753716589));
#26564=CARTESIAN_POINT('Ctrl Pts',(0.9246,-0.0656597737776223,2.19771002099059));
#26565=CARTESIAN_POINT('Ctrl Pts',(0.9246,-0.0613394413265084,2.1954000414296));
#26566=CARTESIAN_POINT('Ctrl Pts',(0.9246,-0.0510345828658487,2.18989027737962));
#26567=CARTESIAN_POINT('Ctrl Pts',(0.9246,-0.0402077092576111,2.18542802572008));
#26568=CARTESIAN_POINT('Ctrl Pts',(0.9246,-0.029053385574336,2.1820750264314));
#26569=CARTESIAN_POINT('Ctrl Pts',(0.9246,-0.0239640761508618,2.18054517564338));
#26570=CARTESIAN_POINT('Ctrl Pts',(0.9246,-0.0188060444905203,2.1792467236037));
#26571=CARTESIAN_POINT('Ctrl Pts',(0.9246,-0.0135956684926093,2.17818840646918));
#26572=CARTESIAN_POINT('Ctrl Pts',(0.9246,-0.0090193919946775,2.17725888586799));
#26573=CARTESIAN_POINT('Ctrl Pts',(0.9246,-0.00439842751910679,2.17651455635539));
#26574=CARTESIAN_POINT('Ctrl Pts',(0.9246,0.000228106976056453,2.17596483471338));
#26575=CARTESIAN_POINT('Ctrl Pts',(0.9246,0.00784207747715569,2.17506014798285));
#26576=CARTESIAN_POINT('Ctrl Pts',(0.9246,0.0154840912914549,2.17467851448771));
#26577=CARTESIAN_POINT('Ctrl Pts',(0.9246,0.0231034225456308,2.17483850328635));
#26578=CARTESIAN_POINT('Ctrl Pts',(0.9246,0.0308943277984289,2.1750020947526));
#26579=CARTESIAN_POINT('Ctrl Pts',(0.9246,0.038661730991992,2.17573174383391));
#26580=CARTESIAN_POINT('Ctrl Pts',(0.9246,0.0463653400536272,2.17699151048238));
#26581=CARTESIAN_POINT('Ctrl Pts',(0.9246,0.0507498095388217,2.1777085001926));
#26582=CARTESIAN_POINT('Ctrl Pts',(0.9246,0.0551136501323604,2.17859740678896));
#26583=CARTESIAN_POINT('Ctrl Pts',(0.9246,0.0594494767860557,2.17965309039764));
#26584=CARTESIAN_POINT('Ctrl Pts',(0.9246,0.0631992337756272,2.18056607823284));
#26585=CARTESIAN_POINT('Ctrl Pts',(0.9246,0.0669204105008384,2.1816021115383));
#26586=CARTESIAN_POINT('Ctrl Pts',(0.9246,0.0706019654180724,2.18275450707801));
#26587=CARTESIAN_POINT('Ctrl Pts',(0.9246,0.0813244048177332,2.18611083113583));
#26588=CARTESIAN_POINT('Ctrl Pts',(0.9246,0.0917275081526179,2.19045541621774));
#26589=CARTESIAN_POINT('Ctrl Pts',(0.9246,0.101696782898373,2.19568714303042));
#26590=CARTESIAN_POINT('Ctrl Pts',(0.9246,0.109000366691416,2.19951995495838));
#26591=CARTESIAN_POINT('Ctrl Pts',(0.9246,0.116071340784156,2.20382979183443));
#26592=CARTESIAN_POINT('Ctrl Pts',(0.9246,0.122862456295835,2.2085889147266));
#26593=CARTESIAN_POINT('Ctrl Pts',(0.9246,0.125551050441307,2.21047304553302));
#26594=CARTESIAN_POINT('Ctrl Pts',(0.9246,0.128194234915945,2.21242684283041));
#26595=CARTESIAN_POINT('Ctrl Pts',(0.9246,0.13078174991918,2.21444248700447));
#26596=CARTESIAN_POINT('Ctrl Pts',(0.9246,0.140899810628574,2.22232433893425));
#26597=CARTESIAN_POINT('Ctrl Pts',(0.9246,0.150200729496614,2.23117056966092));
#26598=CARTESIAN_POINT('Ctrl Pts',(0.9246,0.158522385857352,2.2408616404524));
#26599=CARTESIAN_POINT('Ctrl Pts',(0.9246,0.164709234946706,2.24806659940553));
#26600=CARTESIAN_POINT('Ctrl Pts',(0.9246,0.170354866494887,2.25573972458116));
#26601=CARTESIAN_POINT('Ctrl Pts',(0.9246,0.175382131162755,2.26384741403295));
#26602=CARTESIAN_POINT('Ctrl Pts',(0.9246,-0.1267411102529,2.25945345876159));
#26603=CARTESIAN_POINT('Ctrl Pts',(0.921315099967346,-0.153066813359842,
2.29683117428655));
#26604=CARTESIAN_POINT('Ctrl Pts',(0.914378854565228,-0.172586882197048,
2.4020958249901));
#26605=CARTESIAN_POINT('Ctrl Pts',(0.903791263793647,-0.0580775762076774,
2.52350712786254));
#26606=CARTESIAN_POINT('Ctrl Pts',(0.892837227685257,0.112250391536416,
2.49451043435059));
#26607=CARTESIAN_POINT('Ctrl Pts',(0.881883191576867,0.182481185996413,
2.33668621664117));
#26608=CARTESIAN_POINT('Ctrl Pts',(0.872668908161658,0.104758862680348,
2.2139193569465));
#26609=CARTESIAN_POINT('Ctrl Pts',(0.867105970115912,0.0267685152039638,
2.19471498811069));
#26610=CARTESIAN_POINT('Ctrl Pts',(0.865194377439629,-1.79285551041419E-5,
2.19468551470809));
#26611=CARTESIAN_POINT('Origin',(0.9246,2.59090492670967E-17,2.35));
#26612=CARTESIAN_POINT('',(0.9246,-2.39295984553393E-17,2.1546));
#26613=CARTESIAN_POINT('Origin',(0.9246,0.,2.35));
#26614=CARTESIAN_POINT('Origin',(0.9246,0.,2.35));
#26615=CARTESIAN_POINT('',(0.9246,-0.126612599672286,2.44036067786502));
#26616=CARTESIAN_POINT('Ctrl Pts',(0.9246,0.175579315085692,2.4363567917616));
#26617=CARTESIAN_POINT('Ctrl Pts',(0.9246,0.172231987765182,2.44182477166145));
#26618=CARTESIAN_POINT('Ctrl Pts',(0.9246,0.168608550730546,2.44710587712298));
#26619=CARTESIAN_POINT('Ctrl Pts',(0.9246,0.164708478737988,2.45217506292884));
#26620=CARTESIAN_POINT('Ctrl Pts',(0.9246,0.158764977139952,2.45990023159121));
#26621=CARTESIAN_POINT('Ctrl Pts',(0.9246,0.152179218509756,2.46713401293529));
#26622=CARTESIAN_POINT('Ctrl Pts',(0.9246,0.145034638687745,2.47383351561557));
#26623=CARTESIAN_POINT('Ctrl Pts',(0.9246,0.142072703988846,2.47661093429496));
#26624=CARTESIAN_POINT('Ctrl Pts',(0.9246,0.139016477261661,2.47929437243742));
#26625=CARTESIAN_POINT('Ctrl Pts',(0.9246,0.135878681353299,2.48187551125661));
#26626=CARTESIAN_POINT('Ctrl Pts',(0.9246,0.130129041557607,2.48660514278983));
#26627=CARTESIAN_POINT('Ctrl Pts',(0.9246,0.124099585925552,2.49099741573807));
#26628=CARTESIAN_POINT('Ctrl Pts',(0.9246,0.117828170685741,2.49503327073206));
#26629=CARTESIAN_POINT('Ctrl Pts',(0.9246,0.113097205680066,2.49807779704939));
#26630=CARTESIAN_POINT('Ctrl Pts',(0.9246,0.108228470452361,2.50091938744955));
#26631=CARTESIAN_POINT('Ctrl Pts',(0.9246,0.103237746210791,2.50354755952374));
#26632=CARTESIAN_POINT('Ctrl Pts',(0.9246,0.0995081913357007,2.50551158548419));
#26633=CARTESIAN_POINT('Ctrl Pts',(0.9246,0.095718014229134,2.50735230916665));
#26634=CARTESIAN_POINT('Ctrl Pts',(0.9246,0.0918791218561784,2.50906440216875));
#26635=CARTESIAN_POINT('Ctrl Pts',(0.9246,0.0807315995386604,2.51403604322986));
#26636=CARTESIAN_POINT('Ctrl Pts',(0.9246,0.0691604417837671,2.51793368204044));
#26637=CARTESIAN_POINT('Ctrl Pts',(0.9246,0.0573325104935312,2.52065673448287));
#26638=CARTESIAN_POINT('Ctrl Pts',(0.9246,0.0517514512541242,2.52194161825673));
#26639=CARTESIAN_POINT('Ctrl Pts',(0.9246,0.0461131794767607,2.52296425202055));
#26640=CARTESIAN_POINT('Ctrl Pts',(0.9246,0.0404358087089947,2.52370990579393));
#26641=CARTESIAN_POINT('Ctrl Pts',(0.9246,0.0362131138627409,2.52426450553292));
#26642=CARTESIAN_POINT('Ctrl Pts',(0.9246,0.0319671072283097,2.52466551133679));
#26643=CARTESIAN_POINT('Ctrl Pts',(0.9246,0.0277269183658541,2.52490584661354));
#26644=CARTESIAN_POINT('Ctrl Pts',(0.9246,0.0203386643257472,2.52532461524319));
#26645=CARTESIAN_POINT('Ctrl Pts',(0.9246,0.0129531623571097,2.52525855005896));
#26646=CARTESIAN_POINT('Ctrl Pts',(0.9246,0.00560966548235301,2.52468156733611));
#26647=CARTESIAN_POINT('Ctrl Pts',(0.9246,-0.00111838109498682,2.5241529408929));
#26648=CARTESIAN_POINT('Ctrl Pts',(0.9246,-0.00781125354088175,2.52319524983962));
#26649=CARTESIAN_POINT('Ctrl Pts',(0.9246,-0.0144367695388186,2.52182652343633));
#26650=CARTESIAN_POINT('Ctrl Pts',(0.9246,-0.0194845103225483,2.52078374033993));
#26651=CARTESIAN_POINT('Ctrl Pts',(0.9246,-0.0244931239656314,2.51950225818089));
#26652=CARTESIAN_POINT('Ctrl Pts',(0.9246,-0.0294470198886176,2.51798836500374));
#26653=CARTESIAN_POINT('Ctrl Pts',(0.9246,-0.0327263379688084,2.51698621692787));
#26654=CARTESIAN_POINT('Ctrl Pts',(0.9246,-0.0359767748311459,2.51588354002561));
#26655=CARTESIAN_POINT('Ctrl Pts',(0.9246,-0.0391872039422838,2.5146856379879));
#26656=CARTESIAN_POINT('Ctrl Pts',(0.9246,-0.0483434462127441,2.51126918464356));
#26657=CARTESIAN_POINT('Ctrl Pts',(0.9246,-0.0571935346348361,2.50707428148216));
#26658=CARTESIAN_POINT('Ctrl Pts',(0.9246,-0.0656377525465968,2.50215785253157));
#26659=CARTESIAN_POINT('Ctrl Pts',(0.9246,-0.0707606060416182,2.49917520268812));
#26660=CARTESIAN_POINT('Ctrl Pts',(0.9246,-0.0757337923895695,2.49592655376489));
#26661=CARTESIAN_POINT('Ctrl Pts',(0.9246,-0.0805312179131897,2.4924215291976));
#26662=CARTESIAN_POINT('Ctrl Pts',(0.9246,-0.0832471843025241,2.49043722972872));
#26663=CARTESIAN_POINT('Ctrl Pts',(0.9246,-0.0859085907169423,2.48836919294223));
#26664=CARTESIAN_POINT('Ctrl Pts',(0.9246,-0.0885041357554648,2.4862239808703));
#26665=CARTESIAN_POINT('Ctrl Pts',(0.9246,-0.0968642111344724,2.4793143975808));
#26666=CARTESIAN_POINT('Ctrl Pts',(0.9246,-0.104507209259633,2.47163878643969));
#26667=CARTESIAN_POINT('Ctrl Pts',(0.9246,-0.111283835708874,2.46326800079988));
#26668=CARTESIAN_POINT('Ctrl Pts',(0.9246,-0.117064352600238,2.45612765329108));
#26669=CARTESIAN_POINT('Ctrl Pts',(0.9246,-0.122214313018595,2.44848056071584));
#26670=CARTESIAN_POINT('Ctrl Pts',(0.9246,-0.126612599672285,2.44036067786502));
#26671=CARTESIAN_POINT('Origin',(0.9246,0.,2.35));
#26672=CARTESIAN_POINT('Origin',(1.05400562256037,0.,2.35));
#26673=CARTESIAN_POINT('Ctrl Pts',(0.9246,-0.126612599672285,2.44036067786502));
#26674=CARTESIAN_POINT('Ctrl Pts',(0.920948654630537,-0.096997430212323,
2.48185719696664));
#26675=CARTESIAN_POINT('Ctrl Pts',(0.91364596389161,0.00568860837306084,
2.53282102514772));
#26676=CARTESIAN_POINT('Ctrl Pts',(0.90269192778322,0.155584940979638,2.44648887334014));
#26677=CARTESIAN_POINT('Ctrl Pts',(0.89173789167483,0.166419612567735,2.27405040496673));
#26678=CARTESIAN_POINT('Ctrl Pts',(0.883842456600547,0.0674478883148535,
2.19859243881242));
#26679=CARTESIAN_POINT('Ctrl Pts',(0.879598366895727,0.00838374554634853,
2.19427942878313));
#26680=CARTESIAN_POINT('Ctrl Pts',(0.87900562256037,0.000124190176919186,
2.19434837072514));
#26681=CARTESIAN_POINT('Ctrl Pts',(0.947607408227207,-0.159049193030952,
2.46350997399437));
#26682=CARTESIAN_POINT('Ctrl Pts',(0.943956062857743,-0.121846980800308,
2.51563739175366));
#26683=CARTESIAN_POINT('Ctrl Pts',(0.936653372118817,0.00714595998775946,
2.57965752692937));
#26684=CARTESIAN_POINT('Ctrl Pts',(0.925699336010427,0.19544389242958,2.47120813790205));
#26685=CARTESIAN_POINT('Ctrl Pts',(0.914745299902037,0.209054273839508,
2.25459305130504));
#26686=CARTESIAN_POINT('Ctrl Pts',(0.903791263793647,0.036564329522591,
2.12308336529646));
#26687=CARTESIAN_POINT('Ctrl Pts',(0.892837227685257,-0.168635162060087,
2.19379733502253));
#26688=CARTESIAN_POINT('Ctrl Pts',(0.881883191576868,-0.22346517637455,
2.40375636415297));
#26689=CARTESIAN_POINT('Ctrl Pts',(0.870929155468477,-0.0791446139402059,
2.5657921277133));
#26690=CARTESIAN_POINT('Ctrl Pts',(0.859975119360087,0.135735248705182,
2.53549049134978));
#26691=CARTESIAN_POINT('Ctrl Pts',(0.849021083251697,0.229622539590993,
2.33985357530928));
#26692=CARTESIAN_POINT('Ctrl Pts',(0.838067047143308,0.11884455109742,2.15326158747437));
#26693=CARTESIAN_POINT('Ctrl Pts',(0.827113011034917,-0.0978650376008603,
2.14202768607467));
#26694=CARTESIAN_POINT('Ctrl Pts',(0.816158974926528,-0.227343663615742,
2.31616583232657));
#26695=CARTESIAN_POINT('Ctrl Pts',(0.805204938818137,-0.154184798574543,
2.52046120780869));
#26696=CARTESIAN_POINT('Ctrl Pts',(0.794250902709748,0.0564037123155049,
2.57281963603689));
#26697=CARTESIAN_POINT('Ctrl Pts',(0.783296866601358,0.216717825635759,
2.42657241872938));
#26698=CARTESIAN_POINT('Ctrl Pts',(0.772342830492967,0.183865118597134,
2.21207400158005));
#26699=CARTESIAN_POINT('Ctrl Pts',(0.761388794384579,-0.0128719385109397,
2.12051301962112));
#26700=CARTESIAN_POINT('Ctrl Pts',(0.750434758276188,-0.19813584580039,
2.23350044847083));
#26701=CARTESIAN_POINT('Ctrl Pts',(0.739480722167799,-0.206795533067443,
2.45032730502815));
#26702=CARTESIAN_POINT('Ctrl Pts',(0.728526686059409,-0.031132354710069,
2.57772952623906));
#26703=CARTESIAN_POINT('Ctrl Pts',(0.717572649951018,0.172279990092259,
2.50214980746404));
#26704=CARTESIAN_POINT('Ctrl Pts',(0.706618613842629,0.222134186250392,
2.29095455764139));
#26705=CARTESIAN_POINT('Ctrl Pts',(0.695664577734239,0.0739937252264801,
2.13238820917977));
#26706=CARTESIAN_POINT('Ctrl Pts',(0.684710541625849,-0.140099470470165,
2.16778559433366));
#26707=CARTESIAN_POINT('Ctrl Pts',(0.673756505517459,-0.229317981351449,
2.36559590957524));
#26708=CARTESIAN_POINT('Ctrl Pts',(0.662802469409069,-0.114138643817405,
2.54950525172684));
#26709=CARTESIAN_POINT('Ctrl Pts',(0.651848433300679,0.102775627973098,
2.55558954881783));
#26710=CARTESIAN_POINT('Ctrl Pts',(0.640894397192289,0.228083298654142,
2.37842635782365));
#26711=CARTESIAN_POINT('Ctrl Pts',(0.629940361083899,0.150093116511318,
2.17592505446052));
#26712=CARTESIAN_POINT('Ctrl Pts',(0.618986324975509,-0.0616782521441111,
2.12858352853803));
#26713=CARTESIAN_POINT('Ctrl Pts',(0.60803228886712,-0.218476302610795,
2.27859352046379));
#26714=CARTESIAN_POINT('Ctrl Pts',(0.597078252758729,-0.180535547996485,
2.49225690917627));
#26715=CARTESIAN_POINT('Ctrl Pts',(0.58612421665034,0.0183128246430198,
2.57910930184663));
#26716=CARTESIAN_POINT('Ctrl Pts',(0.57517018054195,0.200856123874476,2.46177615099481));
#26717=CARTESIAN_POINT('Ctrl Pts',(0.564216144433559,0.204335629037752,
2.24476188901181));
#26718=CARTESIAN_POINT('Ctrl Pts',(0.553262108325171,0.0257537850119573,
2.12165176193497));
#26719=CARTESIAN_POINT('Ctrl Pts',(0.542308072216779,-0.17591953461002,
2.20187152493763));
#26720=CARTESIAN_POINT('Ctrl Pts',(0.53135403610839,-0.220517757106366,
2.41454117461156));
#26721=CARTESIAN_POINT('Ctrl Pts',(0.524051345369463,-0.119597839472195,
2.51726861352534));
#26722=CARTESIAN_POINT('Ctrl Pts',(0.5204,-0.0584934195161147,2.53643948045763));
#26723=CARTESIAN_POINT('Ctrl Pts',(0.939938272151471,-0.14823699524473,
2.45579354195125));
#26724=CARTESIAN_POINT('Ctrl Pts',(0.936286926782008,-0.11356379727098,
2.50437732682465));
#26725=CARTESIAN_POINT('Ctrl Pts',(0.928984236043081,0.00666017611619341,
2.56404535966882));
#26726=CARTESIAN_POINT('Ctrl Pts',(0.918030199934691,0.182157575279599,
2.46296838304809));
#26727=CARTESIAN_POINT('Ctrl Pts',(0.907076163826302,0.19484272008225,2.26107883585894));
#26728=CARTESIAN_POINT('Ctrl Pts',(0.896122127717911,0.0340786786671227,
2.13850920612372));
#26729=CARTESIAN_POINT('Ctrl Pts',(0.885168091609522,-0.157171308071526,
2.20441602522955));
#26730=CARTESIAN_POINT('Ctrl Pts',(0.874214055501132,-0.208273966414595,
2.40010199514667));
#26731=CARTESIAN_POINT('Ctrl Pts',(0.863260019392742,-0.0737643463429399,
2.55112253322443));
#26732=CARTESIAN_POINT('Ctrl Pts',(0.852305983284351,0.126507937785869,
2.52288080851067));
#26733=CARTESIAN_POINT('Ctrl Pts',(0.841351947175962,0.214012750777105,
2.34054333140604));
#26734=CARTESIAN_POINT('Ctrl Pts',(0.830397911067572,0.110765473374403,
2.16663590637431));
#26735=CARTESIAN_POINT('Ctrl Pts',(0.819443874959182,-0.0912121516431767,
2.1561656879681));
#26736=CARTESIAN_POINT('Ctrl Pts',(0.808489838850792,-0.211888793272707,
2.31846588620202));
#26737=CARTESIAN_POINT('Ctrl Pts',(0.797535802742403,-0.143703283352442,
2.50887321884387));
#26738=CARTESIAN_POINT('Ctrl Pts',(0.786581766634012,0.0525693760211127,
2.55767231004564));
#26739=CARTESIAN_POINT('Ctrl Pts',(0.775627730525623,0.201985302006306,
2.42136700950665));
#26740=CARTESIAN_POINT('Ctrl Pts',(0.764673694417233,0.171365928941563,
2.22145024012839));
#26741=CARTESIAN_POINT('Ctrl Pts',(0.753719658308842,-0.0119969014081408,
2.13611359309109));
#26742=CARTESIAN_POINT('Ctrl Pts',(0.742765622200453,-0.184666529090828,
2.24142011262716));
#26743=CARTESIAN_POINT('Ctrl Pts',(0.731811586092063,-0.192737528985666,
2.44350703360992));
#26744=CARTESIAN_POINT('Ctrl Pts',(0.720857549983673,-0.0290159706513922,
2.56224842487327));
#26745=CARTESIAN_POINT('Ctrl Pts',(0.709903513875283,0.160568359923073,
2.4918066313681));
#26746=CARTESIAN_POINT('Ctrl Pts',(0.698949477766892,0.207033457280624,
2.29496847930292));
#26747=CARTESIAN_POINT('Ctrl Pts',(0.687995441658504,0.0689636161335506,
2.14718150475157));
#26748=CARTESIAN_POINT('Ctrl Pts',(0.677041405550113,-0.130575478832096,
2.18017256817501));
#26749=CARTESIAN_POINT('Ctrl Pts',(0.666087369441724,-0.213728896471109,
2.36453569634329));
#26750=CARTESIAN_POINT('Ctrl Pts',(0.655133333333333,-0.106379474666734,
2.53594284251273));
#26751=CARTESIAN_POINT('Ctrl Pts',(0.644179297224944,0.0957889190431628,
2.54161352780044));
#26752=CARTESIAN_POINT('Ctrl Pts',(0.633225261116553,0.21257814776474,2.37649392800571));
#26753=CARTESIAN_POINT('Ctrl Pts',(0.622271225008164,0.139889754701397,
2.1877587060807));
#26754=CARTESIAN_POINT('Ctrl Pts',(0.611317188899773,-0.0574853515164367,
2.14363546710466));
#26755=CARTESIAN_POINT('Ctrl Pts',(0.600363152791384,-0.203624237344606,
2.28344774804741));
#26756=CARTESIAN_POINT('Ctrl Pts',(0.589409116682994,-0.168262703254657,
2.48258625439859));
#26757=CARTESIAN_POINT('Ctrl Pts',(0.578455080574604,0.0170679149500409,
2.56353440304317));
#26758=CARTESIAN_POINT('Ctrl Pts',(0.567501044466214,0.187201882086012,
2.45417758460596));
#26759=CARTESIAN_POINT('Ctrl Pts',(0.556547008357824,0.190444849752262,
2.251915998058));
#26760=CARTESIAN_POINT('Ctrl Pts',(0.545592972249434,0.0240030372590971,
2.13717492346157));
#26761=CARTESIAN_POINT('Ctrl Pts',(0.534638936141044,-0.163960487434638,
2.21194133000627));
#26762=CARTESIAN_POINT('Ctrl Pts',(0.523684900032654,-0.205526913331735,
2.41015365190895));
#26763=CARTESIAN_POINT('Ctrl Pts',(0.516382209293728,-0.111467553046117,
2.50589765779524));
#26764=CARTESIAN_POINT('Ctrl Pts',(0.512730863924264,-0.0545170244841849,
2.52376528513823));
#26765=CARTESIAN_POINT('Ctrl Pts',(0.932269136075736,-0.137424797458508,
2.44807710990814));
#26766=CARTESIAN_POINT('Ctrl Pts',(0.928617790706272,-0.105280613741651,
2.49311726189564));
#26767=CARTESIAN_POINT('Ctrl Pts',(0.921315099967346,0.00617439224462701,
2.54843319240827));
#26768=CARTESIAN_POINT('Ctrl Pts',(0.910361063858956,0.168871258129619,
2.45472862819411));
#26769=CARTESIAN_POINT('Ctrl Pts',(0.899407027750566,0.180631166324993,
2.26756462041284));
#26770=CARTESIAN_POINT('Ctrl Pts',(0.888452991642176,0.0315930278116549,
2.15393504695097));
#26771=CARTESIAN_POINT('Ctrl Pts',(0.877498955533787,-0.145707454082965,
2.21503471543656));
#26772=CARTESIAN_POINT('Ctrl Pts',(0.866544919425395,-0.19308275645464,
2.39644762614036));
#26773=CARTESIAN_POINT('Ctrl Pts',(0.855590883317007,-0.068384078745674,
2.53645293873556));
#26774=CARTESIAN_POINT('Ctrl Pts',(0.844636847208615,0.117280626866556,
2.51027112567155));
#26775=CARTESIAN_POINT('Ctrl Pts',(0.833682811100227,0.198402961963217,
2.34123308750281));
#26776=CARTESIAN_POINT('Ctrl Pts',(0.822728774991836,0.102686395651387,
2.18001022527425));
#26777=CARTESIAN_POINT('Ctrl Pts',(0.811774738883446,-0.0845592656854929,
2.17030368986152));
#26778=CARTESIAN_POINT('Ctrl Pts',(0.800820702775057,-0.196433922929672,
2.32076594007746));
#26779=CARTESIAN_POINT('Ctrl Pts',(0.789866666666667,-0.133221768130341,
2.49728522987905));
#26780=CARTESIAN_POINT('Ctrl Pts',(0.778912630558277,0.0487350397267202,
2.54252498405439));
#26781=CARTESIAN_POINT('Ctrl Pts',(0.767958594449887,0.187252778376854,
2.41616160028392));
#26782=CARTESIAN_POINT('Ctrl Pts',(0.757004558341496,0.158866739285992,
2.23082647867672));
#26783=CARTESIAN_POINT('Ctrl Pts',(0.746050522233108,-0.0111218643053415,
2.15171416656106));
#26784=CARTESIAN_POINT('Ctrl Pts',(0.735096486124717,-0.171197212381266,
2.24933977678348));
#26785=CARTESIAN_POINT('Ctrl Pts',(0.724142450016327,-0.178679524903889,
2.43668676219168));
#26786=CARTESIAN_POINT('Ctrl Pts',(0.713188413907937,-0.0268995865927155,
2.54676732350748));
#26787=CARTESIAN_POINT('Ctrl Pts',(0.702234377799547,0.148856729753888,
2.48146345527215));
#26788=CARTESIAN_POINT('Ctrl Pts',(0.691280341691157,0.191932728310855,
2.29898240096446));
#26789=CARTESIAN_POINT('Ctrl Pts',(0.680326305582768,0.0639335070406211,
2.16197480032336));
#26790=CARTESIAN_POINT('Ctrl Pts',(0.669372269474378,-0.121051487194027,
2.19255954201638));
#26791=CARTESIAN_POINT('Ctrl Pts',(0.658418233365988,-0.198139811590769,
2.36347548311133));
#26792=CARTESIAN_POINT('Ctrl Pts',(0.647464197257598,-0.0986203055160625,
2.52238043329861));
#26793=CARTESIAN_POINT('Ctrl Pts',(0.636510161149208,0.0888022101132281,
2.52763750678306));
#26794=CARTESIAN_POINT('Ctrl Pts',(0.625556125040818,0.197072996875337,
2.37456149818778));
#26795=CARTESIAN_POINT('Ctrl Pts',(0.614602088932428,0.129686392891475,
2.19959235770088));
#26796=CARTESIAN_POINT('Ctrl Pts',(0.603648052824039,-0.0532924508887624,
2.15868740567129));
#26797=CARTESIAN_POINT('Ctrl Pts',(0.592694016715648,-0.188772172078417,
2.28830197563102));
#26798=CARTESIAN_POINT('Ctrl Pts',(0.581739980607258,-0.155989858512828,
2.47291559962092));
#26799=CARTESIAN_POINT('Ctrl Pts',(0.570785944498869,0.0158230052570621,
2.54795950423971));
#26800=CARTESIAN_POINT('Ctrl Pts',(0.559831908390478,0.173547640297548,
2.44657901821711));
#26801=CARTESIAN_POINT('Ctrl Pts',(0.548877872282089,0.176554070466772,
2.2590701071042));
#26802=CARTESIAN_POINT('Ctrl Pts',(0.537923836173699,0.022252289506237,
2.15269808498817));
#26803=CARTESIAN_POINT('Ctrl Pts',(0.526969800065309,-0.152001440259255,
2.22201113507491));
#26804=CARTESIAN_POINT('Ctrl Pts',(0.516015763956919,-0.190536069557104,
2.40576612920634));
#26805=CARTESIAN_POINT('Ctrl Pts',(0.508713073217992,-0.103337266620039,
2.49452670206514));
#26806=CARTESIAN_POINT('Ctrl Pts',(0.505061727848529,-0.0505406294522551,
2.51109108981882));
#26807=CARTESIAN_POINT('Ctrl Pts',(0.9246,-0.126612599672285,2.44036067786502));
#26808=CARTESIAN_POINT('Ctrl Pts',(0.920948654630537,-0.096997430212323,
2.48185719696664));
#26809=CARTESIAN_POINT('Ctrl Pts',(0.91364596389161,0.00568860837306084,
2.53282102514772));
#26810=CARTESIAN_POINT('Ctrl Pts',(0.90269192778322,0.155584940979638,2.44648887334014));
#26811=CARTESIAN_POINT('Ctrl Pts',(0.89173789167483,0.166419612567735,2.27405040496673));
#26812=CARTESIAN_POINT('Ctrl Pts',(0.880783855566441,0.0291073769561869,
2.16936088777822));
#26813=CARTESIAN_POINT('Ctrl Pts',(0.86982981945805,-0.134243600094404,
2.22565340564358));
#26814=CARTESIAN_POINT('Ctrl Pts',(0.858875783349661,-0.177891546494684,
2.39279325713406));
#26815=CARTESIAN_POINT('Ctrl Pts',(0.847921747241271,-0.0630038111484079,
2.52178334424669));
#26816=CARTESIAN_POINT('Ctrl Pts',(0.83696771113288,0.108053315947243,2.49766144283244));
#26817=CARTESIAN_POINT('Ctrl Pts',(0.826013675024491,0.18279317314933,2.34192284359958));
#26818=CARTESIAN_POINT('Ctrl Pts',(0.815059638916101,0.0946073179283704,
2.1933845441742));
#26819=CARTESIAN_POINT('Ctrl Pts',(0.804105602807711,-0.0779063797278091,
2.18444169175494));
#26820=CARTESIAN_POINT('Ctrl Pts',(0.793151566699321,-0.180979052586637,
2.32306599395291));
#26821=CARTESIAN_POINT('Ctrl Pts',(0.782197530590931,-0.12274025290824,
2.48569724091423));
#26822=CARTESIAN_POINT('Ctrl Pts',(0.771243494482541,0.0449007034323279,
2.52737765806314));
#26823=CARTESIAN_POINT('Ctrl Pts',(0.760289458374152,0.172520254747402,
2.41095619106118));
#26824=CARTESIAN_POINT('Ctrl Pts',(0.749335422265761,0.146367549630421,
2.24020271722506));
#26825=CARTESIAN_POINT('Ctrl Pts',(0.738381386157372,-0.0102468272025424,
2.16731474003104));
#26826=CARTESIAN_POINT('Ctrl Pts',(0.727427350048981,-0.157727895671703,
2.2572594409398));
#26827=CARTESIAN_POINT('Ctrl Pts',(0.716473313940592,-0.164621520822112,
2.42986649077344));
#26828=CARTESIAN_POINT('Ctrl Pts',(0.705519277832201,-0.0247832025340387,
2.53128622214169));
#26829=CARTESIAN_POINT('Ctrl Pts',(0.694565241723812,0.137145099584703,
2.47112027917621));
#26830=CARTESIAN_POINT('Ctrl Pts',(0.683611205615422,0.176831999341087,
2.30299632262599));
#26831=CARTESIAN_POINT('Ctrl Pts',(0.672657169507032,0.0589033979476915,
2.17676809589516));
#26832=CARTESIAN_POINT('Ctrl Pts',(0.661703133398642,-0.111527495555958,
2.20494651585773));
#26833=CARTESIAN_POINT('Ctrl Pts',(0.650749097290252,-0.182550726710429,
2.36241526987937));
#26834=CARTESIAN_POINT('Ctrl Pts',(0.639795061181862,-0.0908611363653908,
2.5088180240845));
#26835=CARTESIAN_POINT('Ctrl Pts',(0.628841025073472,0.0818155011832931,
2.51366148576568));
#26836=CARTESIAN_POINT('Ctrl Pts',(0.617886988965083,0.181567845985935,
2.37262906836985));
#26837=CARTESIAN_POINT('Ctrl Pts',(0.606932952856693,0.119483031081553,
2.21142600932105));
#26838=CARTESIAN_POINT('Ctrl Pts',(0.595978916748302,-0.049099550261088,
2.17373934423792));
#26839=CARTESIAN_POINT('Ctrl Pts',(0.585024880639913,-0.173920106812228,
2.29315620321465));
#26840=CARTESIAN_POINT('Ctrl Pts',(0.574070844531523,-0.143717013770999,
2.46324494484324));
#26841=CARTESIAN_POINT('Ctrl Pts',(0.563116808423133,0.014578095564083,
2.53238460543625));
#26842=CARTESIAN_POINT('Ctrl Pts',(0.552162772314743,0.159893398509083,
2.43898045182826));
#26843=CARTESIAN_POINT('Ctrl Pts',(0.541208736206353,0.162663291181281,
2.2662242161504));
#26844=CARTESIAN_POINT('Ctrl Pts',(0.530254700097963,0.020501541753377,
2.16822124651476));
#26845=CARTESIAN_POINT('Ctrl Pts',(0.519300663989573,-0.140042393083873,
2.23208094014354));
#26846=CARTESIAN_POINT('Ctrl Pts',(0.508346627881183,-0.175545225782473,
2.40137860650373));
#26847=CARTESIAN_POINT('Ctrl Pts',(0.501043937142257,-0.0952069801939604,
2.48315574633504));
#26848=CARTESIAN_POINT('Ctrl Pts',(0.497392591772793,-0.0465642344203253,
2.49841689449941));
#26849=CARTESIAN_POINT('Ctrl Pts',(0.5204,-0.0584934195161159,2.53643948045763));
#26850=CARTESIAN_POINT('Ctrl Pts',(0.524051345369463,-0.119597839472196,
2.51726861352533));
#26851=CARTESIAN_POINT('Ctrl Pts',(0.527702690738927,-0.170057798289281,
2.46590489406845));
#26852=CARTESIAN_POINT('Ctrl Pts',(0.53135403610839,-0.187854740615099,
2.40477809272768));
#26853=CARTESIAN_POINT('Ctrl Pts',(0.535005381477853,-0.205651682940918,
2.34365129138692));
#26854=CARTESIAN_POINT('Ctrl Pts',(0.538656726847316,-0.190785608775469,
2.27276140816228));
#26855=CARTESIAN_POINT('Ctrl Pts',(0.54230807221678,-0.149740351755748,
2.22394650604951));
#26856=CARTESIAN_POINT('Ctrl Pts',(0.545543058407045,-0.113375443427666,
2.18069791731435));
#26857=CARTESIAN_POINT('Ctrl Pts',(0.548778044597311,-0.056461325508588,
2.15477696695928));
#26858=CARTESIAN_POINT('Ctrl Pts',(0.552013030787577,0.000119548669269599,
2.15439909884273));
#26859=CARTESIAN_POINT('Origin',(0.95,0.0577350269189626,2.45));
#26860=CARTESIAN_POINT('',(0.95,0.0577350269189626,2.45));
#26861=CARTESIAN_POINT('',(0.95,0.115470053837925,2.35));
#26862=CARTESIAN_POINT('',(0.95,0.0353627039878646,2.48875));
#26863=CARTESIAN_POINT('',(0.75,0.0577350269189626,2.45));
#26864=CARTESIAN_POINT('',(0.95,0.0577350269189626,2.45));
#26865=CARTESIAN_POINT('',(0.75,0.115470053837925,2.35));
#26866=CARTESIAN_POINT('',(0.75,0.115470053837925,2.35));
#26867=CARTESIAN_POINT('',(0.95,0.115470053837925,2.35));
#26868=CARTESIAN_POINT('Origin',(0.95,-0.0577350269189626,2.45));
#26869=CARTESIAN_POINT('',(0.95,-0.0577350269189626,2.45));
#26870=CARTESIAN_POINT('',(0.95,-0.0288675134594813,2.45));
#26871=CARTESIAN_POINT('',(0.75,-0.0577350269189626,2.45));
#26872=CARTESIAN_POINT('',(0.95,-0.0577350269189626,2.45));
#26873=CARTESIAN_POINT('',(0.75,0.0577350269189626,2.45));
#26874=CARTESIAN_POINT('Origin',(0.95,-0.115470053837925,2.35));
#26875=CARTESIAN_POINT('',(0.95,-0.115470053837925,2.35));
#26876=CARTESIAN_POINT('',(0.95,-0.0642302174473459,2.43875));
#26877=CARTESIAN_POINT('',(0.75,-0.115470053837925,2.35));
#26878=CARTESIAN_POINT('',(0.95,-0.115470053837925,2.35));
#26879=CARTESIAN_POINT('',(0.75,-0.0577350269189626,2.45));
#26880=CARTESIAN_POINT('Origin',(0.95,-0.0577350269189626,2.25));
#26881=CARTESIAN_POINT('',(0.95,-0.0577350269189626,2.25));
#26882=CARTESIAN_POINT('',(0.95,-0.108974863309542,2.33875));
#26883=CARTESIAN_POINT('',(0.75,-0.0577350269189626,2.25));
#26884=CARTESIAN_POINT('',(0.95,-0.0577350269189626,2.25));
#26885=CARTESIAN_POINT('',(0.75,-0.115470053837925,2.35));
#26886=CARTESIAN_POINT('Origin',(0.95,0.0577350269189626,2.25));
#26887=CARTESIAN_POINT('',(0.95,0.0577350269189626,2.25));
#26888=CARTESIAN_POINT('',(0.95,0.0288675134594813,2.25));
#26889=CARTESIAN_POINT('',(0.75,0.0577350269189626,2.25));
#26890=CARTESIAN_POINT('',(0.95,0.0577350269189626,2.25));
#26891=CARTESIAN_POINT('',(0.75,-0.0577350269189626,2.25));
#26892=CARTESIAN_POINT('Origin',(0.95,0.115470053837925,2.35));
#26893=CARTESIAN_POINT('',(0.95,0.137842376769023,2.38875));
#26894=CARTESIAN_POINT('',(0.75,0.0577350269189626,2.25));
#26895=CARTESIAN_POINT('Origin',(0.75,0.,2.35));
#26896=CARTESIAN_POINT('Origin',(0.95,0.,2.52));
#26897=CARTESIAN_POINT('',(0.95,-2.0818995585505E-17,2.18));
#26898=CARTESIAN_POINT('Origin',(0.95,0.,2.35));
#26899=CARTESIAN_POINT('Origin',(0.935,0.,2.35));
#26900=CARTESIAN_POINT('',(0.935,-2.2655965784226E-17,2.165));
#26901=CARTESIAN_POINT('Origin',(0.7225,0.,2.35));
#26902=CARTESIAN_POINT('Origin',(0.5204,0.,2.35));
#26903=CARTESIAN_POINT('Origin',(0.4875,0.,2.35));
#26904=CARTESIAN_POINT('',(0.45,-1.53080849893419E-17,2.225));
#26905=CARTESIAN_POINT('Origin',(0.45,0.,2.35));
#26906=CARTESIAN_POINT('',(0.4875,-1.99005104861445E-17,2.1875));
#26907=CARTESIAN_POINT('Origin',(0.45,0.,2.35));
#26908=CARTESIAN_POINT('',(0.,0.,0.));
#26909=CARTESIAN_POINT('Origin',(0.,0.,-4.78));
#26910=CARTESIAN_POINT('',(-0.294559949103625,0.000186743463070703,-5.93358238829104));
#26911=CARTESIAN_POINT('',(-0.294471258456466,0.000304903072910924,-5.94801761170896));
#26912=CARTESIAN_POINT('',(-0.2942,-3.60291088309151E-17,-4.78));
#26913=CARTESIAN_POINT('',(0.129048198622908,0.264655422342712,-5.9658));
#26914=CARTESIAN_POINT('Ctrl Pts',(-0.294559949103625,0.000186743463070703,
-5.93358238829104));
#26915=CARTESIAN_POINT('Ctrl Pts',(-0.294627032470039,0.0100023901992575,
-5.93411527799486));
#26916=CARTESIAN_POINT('Ctrl Pts',(-0.294179137669504,0.0198114650280941,
-5.93464816769869));
#26917=CARTESIAN_POINT('Ctrl Pts',(-0.293196168851624,0.0295661465485133,
-5.93518105740251));
#26918=CARTESIAN_POINT('Ctrl Pts',(-0.283428647221269,0.126496039964018,
-5.94047625254401));
#26919=CARTESIAN_POINT('Ctrl Pts',(-0.22082838450258,0.218055185618655,
-5.94577144768552));
#26920=CARTESIAN_POINT('Ctrl Pts',(-0.134050591616501,0.262404015513014,
-5.95106664282702));
#26921=CARTESIAN_POINT('Ctrl Pts',(-0.0535670473776308,0.303536094286101,
-5.95597776188468));
#26922=CARTESIAN_POINT('Ctrl Pts',(0.0477138908823457,0.304058088740004,
-5.96088888094234));
#26923=CARTESIAN_POINT('Ctrl Pts',(0.129204211840496,0.264848286765706,
-5.9658));
#26924=CARTESIAN_POINT('',(-0.128892185405324,0.264462557919717,-5.9658));
#26925=CARTESIAN_POINT('Origin',(0.,0.,-5.9658));
#26926=CARTESIAN_POINT('Ctrl Pts',(-0.128892185405323,0.264462557919717,
-5.9658));
#26927=CARTESIAN_POINT('Ctrl Pts',(-0.216880709330539,0.22157923549964,
-5.9605048048585));
#26928=CARTESIAN_POINT('Ctrl Pts',(-0.281018683526877,0.131692775518941,
-5.955209609717));
#26929=CARTESIAN_POINT('Ctrl Pts',(-0.292556379756586,0.0351079458526411,
-5.94991441457549));
#26930=CARTESIAN_POINT('Ctrl Pts',(-0.293934027145516,0.0235753282701674,
-5.94928214695332));
#26931=CARTESIAN_POINT('Ctrl Pts',(-0.294561735455353,0.0119472098769066,
-5.94864987933114));
#26932=CARTESIAN_POINT('Ctrl Pts',(-0.294471258456466,0.000304903072910924,
-5.94801761170896));
#26933=CARTESIAN_POINT('Origin',(0.,0.,-4.78));
#26934=CARTESIAN_POINT('',(-0.29380273100684,0.000158508790185821,-5.83358238829104));
#26935=CARTESIAN_POINT('',(-0.293774534382448,0.000134529535736241,-5.84801761170896));
#26936=CARTESIAN_POINT('',(-0.2942,-3.60291088309151E-17,-4.78));
#26937=CARTESIAN_POINT('Ctrl Pts',(-0.29380273100684,0.000158508790185821,
-5.83358238829104));
#26938=CARTESIAN_POINT('Ctrl Pts',(-0.293992111209095,0.0390074262588899,
-5.83567744047919));
#26939=CARTESIAN_POINT('Ctrl Pts',(-0.2868348483379,0.0777893022419187,
-5.83777249266733));
#26940=CARTESIAN_POINT('Ctrl Pts',(-0.272003615906625,0.11337249089091,
-5.83986754485547));
#26941=CARTESIAN_POINT('Ctrl Pts',(-0.234518024685059,0.203308163481623,
-5.84516273999698));
#26942=CARTESIAN_POINT('Ctrl Pts',(-0.148010061625874,0.272810181931049,
-5.85045793513847));
#26943=CARTESIAN_POINT('Ctrl Pts',(-0.0521100808352343,0.290040469587057,
-5.85575313027997));
#26944=CARTESIAN_POINT('Ctrl Pts',(0.0437898999554048,0.307270757243064,
-5.86104832542148));
#26945=CARTESIAN_POINT('Ctrl Pts',(0.149081898477497,0.272229314105654,
-5.86634352056299));
#26946=CARTESIAN_POINT('Ctrl Pts',(0.215528969047206,0.200965361943426,
-5.87163871570449));
#26947=CARTESIAN_POINT('Ctrl Pts',(0.281976039616915,0.129701409781198,
-5.87693391084599));
#26948=CARTESIAN_POINT('Ctrl Pts',(0.30957818223424,0.0222149485941525,
-5.88222910598749));
#26949=CARTESIAN_POINT('Ctrl Pts',(0.285692032174072,-0.0722451294262938,
-5.88752430112899));
#26950=CARTESIAN_POINT('Ctrl Pts',(0.261805882113904,-0.16670520744674,
-5.89281949627049));
#26951=CARTESIAN_POINT('Ctrl Pts',(0.186431439376243,-0.248138902300588,
-5.89811469141199));
#26952=CARTESIAN_POINT('Ctrl Pts',(0.0940958433066458,-0.279254488405062,
-5.9034098865535));
#26953=CARTESIAN_POINT('Ctrl Pts',(0.001760247237048,-0.310370074509537,
-5.908705081695));
#26954=CARTESIAN_POINT('Ctrl Pts',(-0.107536502164486,-0.291167551864638,
-5.9140002768365));
#26955=CARTESIAN_POINT('Ctrl Pts',(-0.183717486594243,-0.230415969954001,
-5.919295471978));
#26956=CARTESIAN_POINT('Ctrl Pts',(-0.252231886291065,-0.175778212298382,
-5.92405777741568));
#26957=CARTESIAN_POINT('Ctrl Pts',(-0.293960441403705,-0.0875332997103763,
-5.92882008285336));
#26958=CARTESIAN_POINT('Ctrl Pts',(-0.294559949103625,0.000186743463070703,
-5.93358238829104));
#26959=CARTESIAN_POINT('Ctrl Pts',(-0.294471258456466,0.000304903072910924,
-5.94801761170896));
#26960=CARTESIAN_POINT('Ctrl Pts',(-0.293803997200033,-0.0855562590056137,
-5.94335468418964));
#26961=CARTESIAN_POINT('Ctrl Pts',(-0.254074962086798,-0.172189122321664,
-5.93869175667031));
#26962=CARTESIAN_POINT('Ctrl Pts',(-0.188021191762815,-0.22697774332338,
-5.93402882915099));
#26963=CARTESIAN_POINT('Ctrl Pts',(-0.113010889276256,-0.289195403481199,
-5.92873363400948));
#26964=CARTESIAN_POINT('Ctrl Pts',(-0.00405286604006003,-0.310347524444936,
-5.92343843886798));
#26965=CARTESIAN_POINT('Ctrl Pts',(0.088859077893019,-0.280943894524006,
-5.91814324372648));
#26966=CARTESIAN_POINT('Ctrl Pts',(0.181771021826098,-0.251540264603077,
-5.91284804858498));
#26967=CARTESIAN_POINT('Ctrl Pts',(0.25863688645606,-0.171580883797481,
-5.90755285344348));
#26968=CARTESIAN_POINT('Ctrl Pts',(0.284283196980506,-0.0775964529077967,
-5.90225765830198));
#26969=CARTESIAN_POINT('Ctrl Pts',(0.309929507504952,0.0163879779818879,
-5.89696246316047));
#26970=CARTESIAN_POINT('Ctrl Pts',(0.284356263923882,0.124397458955661,
-5.89166726801896));
#26971=CARTESIAN_POINT('Ctrl Pts',(0.219258296584676,0.196899540204839,
-5.88637207287746));
#26972=CARTESIAN_POINT('Ctrl Pts',(0.154160329245471,0.269401621454017,
-5.88107687773596));
#26973=CARTESIAN_POINT('Ctrl Pts',(0.0495376381481295,0.306396302978599,
-5.87578168259446));
#26974=CARTESIAN_POINT('Ctrl Pts',(-0.0466695936054424,0.290962258147836,
-5.87048648745296));
#26975=CARTESIAN_POINT('Ctrl Pts',(-0.142876825359014,0.275528213317072,
-5.86519129231146));
#26976=CARTESIAN_POINT('Ctrl Pts',(-0.230668597768817,0.207665442130963,
-5.85989609716995));
#26977=CARTESIAN_POINT('Ctrl Pts',(-0.269831522332246,0.118449307439144,
-5.85460090202845));
#26978=CARTESIAN_POINT('Ctrl Pts',(-0.286061387034849,0.0814764354823459,
-5.85240647192195));
#26979=CARTESIAN_POINT('Ctrl Pts',(-0.293939577487073,0.0408362684106601,
-5.85021204181546));
#26980=CARTESIAN_POINT('Ctrl Pts',(-0.293774534382448,0.000134529535736241,
-5.84801761170896));
#26981=CARTESIAN_POINT('Origin',(0.,0.,-4.78));
#26982=CARTESIAN_POINT('',(-0.293985954688873,-0.000246338135983792,-5.73358238829104));
#26983=CARTESIAN_POINT('',(-0.294035653894533,-0.000257348498283876,-5.74801761170896));
#26984=CARTESIAN_POINT('',(-0.2942,-3.60291088309151E-17,-4.78));
#26985=CARTESIAN_POINT('Ctrl Pts',(-0.293985954688873,-0.000246338135983792,
-5.73358238829104));
#26986=CARTESIAN_POINT('Ctrl Pts',(-0.293449964951742,0.0674637013066885,
-5.7372396029635));
#26987=CARTESIAN_POINT('Ctrl Pts',(-0.270196227990946,0.135506165383028,
-5.74089681763597));
#26988=CARTESIAN_POINT('Ctrl Pts',(-0.227393008719715,0.187434463377991,
-5.74455403230843));
#26989=CARTESIAN_POINT('Ctrl Pts',(-0.165419233859773,0.262620225187336,
-5.74984922744993));
#26990=CARTESIAN_POINT('Ctrl Pts',(-0.0624629735245657,0.304025114087145,
-5.75514442259143));
#26991=CARTESIAN_POINT('Ctrl Pts',(0.0343097335839951,0.292680871287088,
-5.76043961773294));
#26992=CARTESIAN_POINT('Ctrl Pts',(0.131082440692556,0.281336628487032,
-5.76573481287444));
#26993=CARTESIAN_POINT('Ctrl Pts',(0.22167159457447,0.217243253987109,-5.77103000801594));
#26994=CARTESIAN_POINT('Ctrl Pts',(0.26457671740946,0.129762959220209,-5.77632520315744));
#26995=CARTESIAN_POINT('Ctrl Pts',(0.307481840244449,0.0422826644533097,
-5.78162039829895));
#26996=CARTESIAN_POINT('Ctrl Pts',(0.302702932032513,-0.0685845505805679,
-5.78691559344045));
#26997=CARTESIAN_POINT('Ctrl Pts',(0.252429325191917,-0.15204834975367,
-5.79221078858195));
#26998=CARTESIAN_POINT('Ctrl Pts',(0.202155718351321,-0.235512148926771,
-5.79750598372345));
#26999=CARTESIAN_POINT('Ctrl Pts',(0.106387412882064,-0.291572532239098,
-5.80280117886496));
#27000=CARTESIAN_POINT('Ctrl Pts',(0.00899746792928702,-0.294547543830657,
-5.80809637400646));
#27001=CARTESIAN_POINT('Ctrl Pts',(-0.0883924770234898,-0.297522555422217,
-5.81339156914796));
#27002=CARTESIAN_POINT('Ctrl Pts',(-0.187404061459786,-0.24741219529301,
-5.81868676428946));
#27003=CARTESIAN_POINT('Ctrl Pts',(-0.242678243985961,-0.167172351862406,
-5.82398195943096));
#27004=CARTESIAN_POINT('Ctrl Pts',(-0.276083110282096,-0.118679527203212,
-5.82718210238432));
#27005=CARTESIAN_POINT('Ctrl Pts',(-0.293513457201069,-0.0591822991317833,
-5.83038224533768));
#27006=CARTESIAN_POINT('Ctrl Pts',(-0.29380273100684,0.000158508790185821,
-5.83358238829104));
#27007=CARTESIAN_POINT('Ctrl Pts',(-0.293774534382448,0.000134529535736241,
-5.84801761170896));
#27008=CARTESIAN_POINT('Ctrl Pts',(-0.293541325821111,-0.0573776821285201,
-5.84491684667396));
#27009=CARTESIAN_POINT('Ctrl Pts',(-0.277248880893283,-0.115012828945004,
-5.84181608163895));
#27010=CARTESIAN_POINT('Ctrl Pts',(-0.245767387391927,-0.162598270025468,
-5.83871531660395));
#27011=CARTESIAN_POINT('Ctrl Pts',(-0.192006251171125,-0.243860214600734,
-5.83342012146245));
#27012=CARTESIAN_POINT('Ctrl Pts',(-0.0939499020124678,-0.295814605553739,
-5.82812492632094));
#27013=CARTESIAN_POINT('Ctrl Pts',(0.00347886280310267,-0.294663916819073,
-5.82282973117944));
#27014=CARTESIAN_POINT('Ctrl Pts',(0.100907627618673,-0.293513228084406,
-5.81753453603794));
#27015=CARTESIAN_POINT('Ctrl Pts',(0.197708808091157,-0.239257459662068,
-5.81223934089643));
#27016=CARTESIAN_POINT('Ctrl Pts',(0.249536873817293,-0.156750214773644,
-5.80694414575493));
#27017=CARTESIAN_POINT('Ctrl Pts',(0.30136493954343,-0.0742429698852198,
-5.80164895061343));
#27018=CARTESIAN_POINT('Ctrl Pts',(0.308219890523219,0.036515751469291,
-5.79635375547193));
#27019=CARTESIAN_POINT('Ctrl Pts',(0.266960957499969,0.12478447396498,-5.79105856033042));
#27020=CARTESIAN_POINT('Ctrl Pts',(0.22570202447672,0.213053196460669,-5.78576336518892));
#27021=CARTESIAN_POINT('Ctrl Pts',(0.136329207450433,0.278831920097537,
-5.78046817004742));
#27022=CARTESIAN_POINT('Ctrl Pts',(0.0397859484585213,0.291986781501344,
-5.77517297490592));
#27023=CARTESIAN_POINT('Ctrl Pts',(-0.0567573105333909,0.30514164290515,
-5.76987777976442));
#27024=CARTESIAN_POINT('Ctrl Pts',(-0.160471011490928,0.265672642075894,
-5.76458258462291));
#27025=CARTESIAN_POINT('Ctrl Pts',(-0.223842216941555,0.191660948472357,
-5.75928738948141));
#27026=CARTESIAN_POINT('Ctrl Pts',(-0.26879991812259,0.139154520966846,
-5.75553079689059));
#27027=CARTESIAN_POINT('Ctrl Pts',(-0.293453366349353,0.0692628632469418,
-5.75177420429978));
#27028=CARTESIAN_POINT('Ctrl Pts',(-0.294035653894533,-0.000257348498283876,
-5.74801761170896));
#27029=CARTESIAN_POINT('Origin',(0.,0.,-4.78));
#27030=CARTESIAN_POINT('',(-0.294682139675626,-2.60825238454776E-5,-5.63358238829104));
#27031=CARTESIAN_POINT('',(-0.294684718001967,8.11877721581833E-6,-5.64801761170896));
#27032=CARTESIAN_POINT('',(-0.2942,-3.60291088309151E-17,-4.78));
#27033=CARTESIAN_POINT('Ctrl Pts',(-0.294682139675626,-2.60825238454776E-5,
-5.63358238829104));
#27034=CARTESIAN_POINT('Ctrl Pts',(-0.294560459013795,0.0960166948008084,
-5.63880176544782));
#27035=CARTESIAN_POINT('Ctrl Pts',(-0.243173253454164,0.192171161974052,
-5.6440211426046));
#27036=CARTESIAN_POINT('Ctrl Pts',(-0.163207802563854,0.245361916625028,
-5.64924051976138));
#27037=CARTESIAN_POINT('Ctrl Pts',(-0.0820807534307584,0.299325333550112,
-5.65453571490289));
#27038=CARTESIAN_POINT('Ctrl Pts',(0.0284608409375124,0.309067768716717,
-5.6598309100444));
#27039=CARTESIAN_POINT('Ctrl Pts',(0.117775960523091,0.270126044465011,
-5.6651261051859));
#27040=CARTESIAN_POINT('Ctrl Pts',(0.20709108010867,0.231184320213304,-5.6704213003274));
#27041=CARTESIAN_POINT('Ctrl Pts',(0.275179724911557,0.143558436543284,
-5.6757164954689));
#27042=CARTESIAN_POINT('Ctrl Pts',(0.29084930638562,0.0473913279882392,
-5.6810116906104));
#27043=CARTESIAN_POINT('Ctrl Pts',(0.306518887859683,-0.0487757805668053,
-5.6863068857519));
#27044=CARTESIAN_POINT('Ctrl Pts',(0.269769406004923,-0.153484114006876,
-5.69160208089341));
#27045=CARTESIAN_POINT('Ctrl Pts',(0.197436435974479,-0.218764967327266,
-5.69689727603491));
#27046=CARTESIAN_POINT('Ctrl Pts',(0.125103465944034,-0.284045820647656,
-5.70219247117641));
#27047=CARTESIAN_POINT('Ctrl Pts',(0.0171870077379044,-0.309899193848366,
-5.70748766631791));
#27048=CARTESIAN_POINT('Ctrl Pts',(-0.0768745400119588,-0.284481213918727,
-5.71278286145941));
#27049=CARTESIAN_POINT('Ctrl Pts',(-0.170936087761821,-0.259063233989088,
-5.71807805660091));
#27050=CARTESIAN_POINT('Ctrl Pts',(-0.251142725055418,-0.182373900929101,
-5.72337325174242));
#27051=CARTESIAN_POINT('Ctrl Pts',(-0.280750399009877,-0.0895459170396675,
-5.72866844688392));
#27052=CARTESIAN_POINT('Ctrl Pts',(-0.289909040075056,-0.0608311255111185,
-5.73030642735296));
#27053=CARTESIAN_POINT('Ctrl Pts',(-0.294226011890775,-0.0305720729089783,
-5.731944407822));
#27054=CARTESIAN_POINT('Ctrl Pts',(-0.293985954688873,-0.000246338135983792,
-5.73358238829104));
#27055=CARTESIAN_POINT('Ctrl Pts',(-0.294035653894533,-0.000257348498283876,
-5.74801761170896));
#27056=CARTESIAN_POINT('Ctrl Pts',(-0.294274143717581,-0.0287310177955373,
-5.74647900915827));
#27057=CARTESIAN_POINT('Ctrl Pts',(-0.290474676140753,-0.0571423767188976,
-5.74494040660759));
#27058=CARTESIAN_POINT('Ctrl Pts',(-0.28237844057963,-0.084271428370518,
-5.7434018040569));
#27059=CARTESIAN_POINT('Ctrl Pts',(-0.254514748823363,-0.17763772523204,
-5.7381066089154));
#27060=CARTESIAN_POINT('Ctrl Pts',(-0.175758655367114,-0.255815932577267,
-5.7328114137739));
#27061=CARTESIAN_POINT('Ctrl Pts',(-0.0821897200362796,-0.282991329357579,
-5.7275162186324));
#27062=CARTESIAN_POINT('Ctrl Pts',(0.011379215294555,-0.310166726137891,
-5.72222102349089));
#27063=CARTESIAN_POINT('Ctrl Pts',(0.119760992499974,-0.286339312353287,
-5.71692582834939));
#27064=CARTESIAN_POINT('Ctrl Pts',(0.193304055814128,-0.222424802657665,
-5.71163063320789));
#27065=CARTESIAN_POINT('Ctrl Pts',(0.266847119128281,-0.158510292962043,
-5.70633543806639));
#27066=CARTESIAN_POINT('Ctrl Pts',(0.305551468551169,-0.0545086873554045,
-5.70104024292489));
#27067=CARTESIAN_POINT('Ctrl Pts',(0.291685963198157,0.0419350572632446,
-5.69574504778339));
#27068=CARTESIAN_POINT('Ctrl Pts',(0.277820457845145,0.138378801881894,
-5.69044985264189));
#27069=CARTESIAN_POINT('Ctrl Pts',(0.211385097716233,0.227264685512553,
-5.68515465750038));
#27070=CARTESIAN_POINT('Ctrl Pts',(0.122815076627005,0.267872554166424,
-5.67985946235887));
#27071=CARTESIAN_POINT('Ctrl Pts',(0.0342450555377765,0.308480422820294,
-5.67456426721737));
#27072=CARTESIAN_POINT('Ctrl Pts',(-0.0764596265117672,0.300810276497374,
-5.66926907207587));
#27073=CARTESIAN_POINT('Ctrl Pts',(-0.158583238089704,0.248375937095584,
-5.66397387693437));
#27074=CARTESIAN_POINT('Ctrl Pts',(-0.240706849667642,0.195941597693793,
-5.65867868179287));
#27075=CARTESIAN_POINT('Ctrl Pts',(-0.294249390773972,0.0987430652131304,
-5.65338348665136));
#27076=CARTESIAN_POINT('Ctrl Pts',(-0.294682094323317,0.00130867455497656,
-5.64808829150986));
#27077=CARTESIAN_POINT('Ctrl Pts',(-0.294684019553008,0.000875159317817163,
-5.64806473157622));
#27078=CARTESIAN_POINT('Ctrl Pts',(-0.294684893404035,0.000441639411536826,
-5.64804117164259));
#27079=CARTESIAN_POINT('Ctrl Pts',(-0.294684718001967,8.11877721581833E-6,
-5.64801761170896));
#27080=CARTESIAN_POINT('Origin',(0.,0.,-4.78));
#27081=CARTESIAN_POINT('',(-0.294062830248701,0.000261802542909251,-5.53358238829104));
#27082=CARTESIAN_POINT('',(-0.294011745337965,0.000252542567362749,-5.54801761170896));
#27083=CARTESIAN_POINT('',(-0.2942,-3.60291088309151E-17,-4.78));
#27084=CARTESIAN_POINT('Ctrl Pts',(-0.294062830248701,0.000261802542909251,
-5.53358238829104));
#27085=CARTESIAN_POINT('Ctrl Pts',(-0.294298842664649,0.0277619258901645,
-5.53506873279064));
#27086=CARTESIAN_POINT('Ctrl Pts',(-0.290757561165195,0.0552024351269035,
-5.53655507729024));
#27087=CARTESIAN_POINT('Ctrl Pts',(-0.28319483979987,0.081485824609101,
-5.53804142178984));
#27088=CARTESIAN_POINT('Ctrl Pts',(-0.256252172443144,0.175122041734979,
-5.54333661693134));
#27089=CARTESIAN_POINT('Ctrl Pts',(-0.178269987897413,0.254072266884979,
-5.54863181207284));
#27090=CARTESIAN_POINT('Ctrl Pts',(-0.084973276416993,0.282168033621128,
-5.55392700721435));
#27091=CARTESIAN_POINT('Ctrl Pts',(0.00832343506342488,0.310263800357276,
-5.55922220235585));
#27092=CARTESIAN_POINT('Ctrl Pts',(0.116934673478531,0.287505108679576,
-5.56451739749735));
#27093=CARTESIAN_POINT('Ctrl Pts',(0.191103748167855,0.224318109691484,
-5.56981259263885));
#27094=CARTESIAN_POINT('Ctrl Pts',(0.265272822857179,0.161131110703392,
-5.57510778778036));
#27095=CARTESIAN_POINT('Ctrl Pts',(0.304999733820722,0.0575158044049082,
-5.58040298292186));
#27096=CARTESIAN_POINT('Ctrl Pts',(0.29208489463139,-0.0390598416549937,
-5.58569817806336));
#27097=CARTESIAN_POINT('Ctrl Pts',(0.279170055442058,-0.135635487714897,
-5.59099337320486));
#27098=CARTESIAN_POINT('Ctrl Pts',(0.213613466099853,-0.225171473536216,
-5.59628856834637));
#27099=CARTESIAN_POINT('Ctrl Pts',(0.125447736357934,-0.266649812209754,
-5.60158376348787));
#27100=CARTESIAN_POINT('Ctrl Pts',(0.0372820066160163,-0.308128150883291,
-5.60687895862937));
#27101=CARTESIAN_POINT('Ctrl Pts',(-0.0734928635256134,-0.301548842409048,
-5.61217415377087));
#27102=CARTESIAN_POINT('Ctrl Pts',(-0.156128986234019,-0.249925982127323,
-5.61746934891237));
#27103=CARTESIAN_POINT('Ctrl Pts',(-0.238765108942426,-0.198303121845597,
-5.62276454405388));
#27104=CARTESIAN_POINT('Ctrl Pts',(-0.293262484217608,-0.101636709756389,
-5.62805973919538));
#27105=CARTESIAN_POINT('Ctrl Pts',(-0.294654919906238,-0.00421130437000306,
-5.63335493433688));
#27106=CARTESIAN_POINT('Ctrl Pts',(-0.294674857163496,-0.002816342012704,
-5.6334307523216));
#27107=CARTESIAN_POINT('Ctrl Pts',(-0.29468390723951,-0.00142122405222277,
-5.63350657030632));
#27108=CARTESIAN_POINT('Ctrl Pts',(-0.294682139675626,-2.60825238454776E-5,
-5.63358238829104));
#27109=CARTESIAN_POINT('Ctrl Pts',(-0.294684718001967,8.11877721581833E-6,
-5.64801761170896));
#27110=CARTESIAN_POINT('Ctrl Pts',(-0.294645471044368,-0.0969939642816139,
-5.64274597650109));
#27111=CARTESIAN_POINT('Ctrl Pts',(-0.242074357435456,-0.194032497397622,
-5.63747434129323));
#27112=CARTESIAN_POINT('Ctrl Pts',(-0.160783000885537,-0.246957639589329,
-5.63220270608536));
#27113=CARTESIAN_POINT('Ctrl Pts',(-0.0791283379060545,-0.300119314239834,
-5.62690751094386));
#27114=CARTESIAN_POINT('Ctrl Pts',(0.0315038540452678,-0.308772414705198,
-5.62161231580235));
#27115=CARTESIAN_POINT('Ctrl Pts',(0.120431050747587,-0.268952804993428,
-5.61631712066085));
#27116=CARTESIAN_POINT('Ctrl Pts',(0.209358247449906,-0.229133195281657,
-5.61102192551934));
#27117=CARTESIAN_POINT('Ctrl Pts',(0.276580448903222,-0.140840875392752,
-5.60572673037785));
#27118=CARTESIAN_POINT('Ctrl Pts',(0.291301999444768,-0.0445240876285061,
-5.60043153523634));
#27119=CARTESIAN_POINT('Ctrl Pts',(0.306023549986313,0.0517927001357388,
-5.59513634009484));
#27120=CARTESIAN_POINT('Ctrl Pts',(0.268244449616089,0.156133955775324,
-5.58984114495334));
#27121=CARTESIAN_POINT('Ctrl Pts',(0.195271959040515,0.220699141927202,
-5.58454594981184));
#27122=CARTESIAN_POINT('Ctrl Pts',(0.12229946846494,0.285264328079082,-5.57925075467033));
#27123=CARTESIAN_POINT('Ctrl Pts',(0.0141335876840122,0.310053444743254,
-5.57395555952883));
#27124=CARTESIAN_POINT('Ctrl Pts',(-0.0796730187285941,0.28371016785751,
-5.56866036438733));
#27125=CARTESIAN_POINT('Ctrl Pts',(-0.1734796251412,0.257366890971767,-5.56336516924582));
#27126=CARTESIAN_POINT('Ctrl Pts',(-0.252926957185485,0.179891220536109,
-5.55806997410432));
#27127=CARTESIAN_POINT('Ctrl Pts',(-0.281618815126852,0.0867761039612887,
-5.55277477896282));
#27128=CARTESIAN_POINT('Ctrl Pts',(-0.290211005052726,0.0588914417614489,
-5.55118905654487));
#27129=CARTESIAN_POINT('Ctrl Pts',(-0.294251498631625,0.0296042508468538,
-5.54960333412692));
#27130=CARTESIAN_POINT('Ctrl Pts',(-0.294011745337965,0.000252542567362749,
-5.54801761170896));
#27131=CARTESIAN_POINT('Origin',(0.,0.,-4.78));
#27132=CARTESIAN_POINT('',(-0.293762945406406,-0.000118368460801849,-5.43358238829104));
#27133=CARTESIAN_POINT('',(-0.293787729549656,-0.000144936987199139,-5.44801761170896));
#27134=CARTESIAN_POINT('',(-0.2942,-3.60291088309151E-17,-4.78));
#27135=CARTESIAN_POINT('Ctrl Pts',(-0.293762945406406,-0.000118368460801849,
-5.43358238829104));
#27136=CARTESIAN_POINT('Ctrl Pts',(-0.29355838126358,0.0564296933406882,
-5.43663089527496));
#27137=CARTESIAN_POINT('Ctrl Pts',(-0.27784549825086,0.113082938218205,
-5.43967940225888));
#27138=CARTESIAN_POINT('Ctrl Pts',(-0.247356669228761,0.160168458472912,
-5.4427279092428));
#27139=CARTESIAN_POINT('Ctrl Pts',(-0.194398188188848,0.241955057422185,
-5.4480231043843));
#27140=CARTESIAN_POINT('Ctrl Pts',(-0.0968592162767127,0.29487488466396,
-5.4533182995258));
#27141=CARTESIAN_POINT('Ctrl Pts',(0.00057595302291618,0.294684450183038,
-5.4586134946673));
#27142=CARTESIAN_POINT('Ctrl Pts',(0.0980111223225464,0.294494015702115,
-5.4639086898088));
#27143=CARTESIAN_POINT('Ctrl Pts',(0.19534248900967,0.241193319498494,-5.46920388495031));
#27144=CARTESIAN_POINT('Ctrl Pts',(0.247980867151239,0.159200334259781,
-5.47449908009182));
#27145=CARTESIAN_POINT('Ctrl Pts',(0.300619245292808,0.0772073490210695,
-5.47979427523332));
#27146=CARTESIAN_POINT('Ctrl Pts',(0.308564634888824,-0.033477925252733,
-5.48508947037482));
#27147=CARTESIAN_POINT('Ctrl Pts',(0.268177115263378,-0.122148646126489,
-5.49038466551632));
#27148=CARTESIAN_POINT('Ctrl Pts',(0.227789595637931,-0.210819367000247,
-5.49567986065782));
#27149=CARTESIAN_POINT('Ctrl Pts',(0.13906916679102,-0.277475534473958,
-5.50097505579933));
#27150=CARTESIAN_POINT('Ctrl Pts',(0.0426601947948733,-0.291580803006248,
-5.50627025094083));
#27151=CARTESIAN_POINT('Ctrl Pts',(-0.0537487772012731,-0.305686071538539,
-5.51156544608233));
#27152=CARTESIAN_POINT('Ctrl Pts',(-0.157846292346655,-0.26724044112941,
-5.51686064122383));
#27153=CARTESIAN_POINT('Ctrl Pts',(-0.221943474835486,-0.193856521373968,
-5.52215583636533));
#27154=CARTESIAN_POINT('Ctrl Pts',(-0.26804878127703,-0.141071235393637,
-5.52596468700723));
#27155=CARTESIAN_POINT('Ctrl Pts',(-0.293458033687594,-0.0702089816473159,
-5.52977353764913));
#27156=CARTESIAN_POINT('Ctrl Pts',(-0.294062830248701,0.000261802542909251,
-5.53358238829104));
#27157=CARTESIAN_POINT('Ctrl Pts',(-0.294011745337965,0.000252542567362749,
-5.54801761170896));
#27158=CARTESIAN_POINT('Ctrl Pts',(-0.293450891626658,-0.0684097655514012,
-5.54430813898541));
#27159=CARTESIAN_POINT('Ctrl Pts',(-0.269467235735366,-0.137425132154906,
-5.54059866626186));
#27160=CARTESIAN_POINT('Ctrl Pts',(-0.225535691601695,-0.18966523419781,
-5.53688919353831));
#27161=CARTESIAN_POINT('Ctrl Pts',(-0.162824326296723,-0.264236893068108,
-5.53159399839681));
#27162=CARTESIAN_POINT('Ctrl Pts',(-0.0594652118483327,-0.304625648094722,
-5.52629880325531));
#27163=CARTESIAN_POINT('Ctrl Pts',(0.0371910500992316,-0.292328710607396,
-5.52100360811381));
#27164=CARTESIAN_POINT('Ctrl Pts',(0.133847312046796,-0.28003177312007,
-5.51570841297231));
#27165=CARTESIAN_POINT('Ctrl Pts',(0.223800721493533,-0.215049143118806,
-5.5104132178308));
#27166=CARTESIAN_POINT('Ctrl Pts',(0.265842062583014,-0.127150489630659,
-5.5051180226893));
#27167=CARTESIAN_POINT('Ctrl Pts',(0.307883403672496,-0.0392518361425124,
-5.4998228275478));
#27168=CARTESIAN_POINT('Ctrl Pts',(0.302012676404721,0.0715628408325163,
-5.4945276324063));
#27169=CARTESIAN_POINT('Ctrl Pts',(0.250919362688317,0.154527417242256,
-5.48923243726479));
#27170=CARTESIAN_POINT('Ctrl Pts',(0.199826048971912,0.237491993651996,
-5.48393724212329));
#27171=CARTESIAN_POINT('Ctrl Pts',(0.103510148806877,0.292606469496448,
-5.47864204698179));
#27172=CARTESIAN_POINT('Ctrl Pts',(0.00609564531270745,0.294621948198257,
-5.47334685184029));
#27173=CARTESIAN_POINT('Ctrl Pts',(-0.0913188581814613,0.296637426900067,
-5.46805165669878));
#27174=CARTESIAN_POINT('Ctrl Pts',(-0.189831965004765,0.245553908459236,
-5.46275646155728));
#27175=CARTESIAN_POINT('Ctrl Pts',(-0.244313113586537,0.164773638004936,
-5.45746126641578));
#27176=CARTESIAN_POINT('Ctrl Pts',(-0.276701038959653,0.116751424097918,
-5.45431338151351));
#27177=CARTESIAN_POINT('Ctrl Pts',(-0.29352781213388,0.0582342039193331,
-5.45116549661124));
#27178=CARTESIAN_POINT('Ctrl Pts',(-0.293787729549656,-0.000144936987199139,
-5.44801761170896));
#27179=CARTESIAN_POINT('Origin',(0.,0.,-4.78));
#27180=CARTESIAN_POINT('',(-0.294496711936401,-0.000204427085817055,-5.33358238829104));
#27181=CARTESIAN_POINT('',(-0.294542023011264,-0.000181426215594961,-5.34801761170896));
#27182=CARTESIAN_POINT('',(-0.2942,-3.60291088309151E-17,-4.78));
#27183=CARTESIAN_POINT('Ctrl Pts',(-0.294496711936401,-0.000204427085817055,
-5.33358238829104));
#27184=CARTESIAN_POINT('Ctrl Pts',(-0.293823771455211,0.084778691105119,
-5.33819305775928));
#27185=CARTESIAN_POINT('Ctrl Pts',(-0.255021031632015,0.170297643646105,
-5.34280372722752));
#27186=CARTESIAN_POINT('Ctrl Pts',(-0.190225443788733,0.225063407591993,
-5.34741439669576));
#27187=CARTESIAN_POINT('Ctrl Pts',(-0.115809942026555,0.287960001929239,
-5.35270959183726));
#27188=CARTESIAN_POINT('Ctrl Pts',(-0.00711057119819164,0.310293965717217,
-5.35800478697876));
#27189=CARTESIAN_POINT('Ctrl Pts',(0.0860756030468191,0.281833723073849,
-5.36329998212026));
#27190=CARTESIAN_POINT('Ctrl Pts',(0.179261777291827,0.253373480430482,
-5.36859517726177));
#27191=CARTESIAN_POINT('Ctrl Pts',(0.256934754953484,0.174119031355772,
-5.37389037240327));
#27192=CARTESIAN_POINT('Ctrl Pts',(0.283511198811562,0.0803782125328151,
-5.37918556754477));
#27193=CARTESIAN_POINT('Ctrl Pts',(0.310087642669642,-0.0133626062901439,
-5.38448076268627));
#27194=CARTESIAN_POINT('Ctrl Pts',(0.285567552724141,-0.121589794861351,
-5.38977595782778));
#27195=CARTESIAN_POINT('Ctrl Pts',(0.221184007137732,-0.194722602406693,
-5.39507115296928));
#27196=CARTESIAN_POINT('Ctrl Pts',(0.156800461551325,-0.267855409952034,
-5.40036634811078));
#27197=CARTESIAN_POINT('Ctrl Pts',(0.052553460324011,-0.305893836471511,
-5.40566154325228));
#27198=CARTESIAN_POINT('Ctrl Pts',(-0.0437996385731037,-0.29141181953107,
-5.41095673839378));
#27199=CARTESIAN_POINT('Ctrl Pts',(-0.140152737470219,-0.276929802590629,
-5.41625193353528));
#27200=CARTESIAN_POINT('Ctrl Pts',(-0.228611934037135,-0.209927342190269,
-5.42154712867679));
#27201=CARTESIAN_POINT('Ctrl Pts',(-0.268652537236749,-0.121099426661703,
-5.42684232381829));
#27202=CARTESIAN_POINT('Ctrl Pts',(-0.28564128772226,-0.0834108013045968,
-5.42908901197587));
#27203=CARTESIAN_POINT('Ctrl Pts',(-0.293913705053531,-0.0417931494122248,
-5.43133570013346));
#27204=CARTESIAN_POINT('Ctrl Pts',(-0.293762945406406,-0.000118368460801849,
-5.43358238829104));
#27205=CARTESIAN_POINT('Ctrl Pts',(-0.293787729549656,-0.000144936987199139,
-5.44801761170896));
#27206=CARTESIAN_POINT('Ctrl Pts',(-0.293965030609122,-0.039967907304658,
-5.44587030146973));
#27207=CARTESIAN_POINT('Ctrl Pts',(-0.286433439129297,-0.0797266265484263,
-5.4437229912305));
#27208=CARTESIAN_POINT('Ctrl Pts',(-0.270873729417273,-0.11604599072477,
-5.44157568099127));
#27209=CARTESIAN_POINT('Ctrl Pts',(-0.232504006325994,-0.205608326532409,
-5.43628048584977));
#27210=CARTESIAN_POINT('Ctrl Pts',(-0.145315369803193,-0.27425597567992,
-5.43098529070827));
#27211=CARTESIAN_POINT('Ctrl Pts',(-0.0492504453095419,-0.290540260357468,
-5.42569009556676));
#27212=CARTESIAN_POINT('Ctrl Pts',(0.0468144791841089,-0.306824545035016,
-5.42039490042526));
#27213=CARTESIAN_POINT('Ctrl Pts',(0.15175569164861,-0.270745465242601,
-5.41509970528376));
#27214=CARTESIAN_POINT('Ctrl Pts',(0.217497803913647,-0.19883147272121,
-5.40980451014226));
#27215=CARTESIAN_POINT('Ctrl Pts',(0.283239916178685,-0.126917480199819,
-5.40450931500076));
#27216=CARTESIAN_POINT('Ctrl Pts',(0.30978292824426,-0.0191685749494507,
-5.39921411985926));
#27217=CARTESIAN_POINT('Ctrl Pts',(0.284967026265175,0.0750536021342638,
-5.39391892471775));
#27218=CARTESIAN_POINT('Ctrl Pts',(0.26015112428609,0.169275779217978,-5.38862372957625));
#27219=CARTESIAN_POINT('Ctrl Pts',(0.183976308262347,0.249971228135038,
-5.38332853443475));
#27220=CARTESIAN_POINT('Ctrl Pts',(0.0913395816031329,0.280171965200513,
-5.37803333929324));
#27221=CARTESIAN_POINT('Ctrl Pts',(-0.00129714505608075,0.310372702265987,
-5.37273814415174));
#27222=CARTESIAN_POINT('Ctrl Pts',(-0.110395782350765,0.290078727479875,
-5.36744294901024));
#27223=CARTESIAN_POINT('Ctrl Pts',(-0.185976353743453,0.228587062407386,
-5.36214775386874));
#27224=CARTESIAN_POINT('Ctrl Pts',(-0.253204862467365,0.173890559515195,
-5.35743770648215));
#27225=CARTESIAN_POINT('Ctrl Pts',(-0.293913856983524,0.0865984189131595,
-5.35272765909555));
#27226=CARTESIAN_POINT('Ctrl Pts',(-0.294542023011264,-0.000181426215594961,
-5.34801761170896));
#27227=CARTESIAN_POINT('Origin',(0.,0.,-4.78));
#27228=CARTESIAN_POINT('',(-0.294398673878215,0.000239804230613712,-5.23358238829104));
#27229=CARTESIAN_POINT('',(-0.294344694043696,0.00025285010085293,-5.24801761170896));
#27230=CARTESIAN_POINT('',(-0.2942,-3.60291088309151E-17,-4.78));
#27231=CARTESIAN_POINT('Ctrl Pts',(-0.294398673878215,0.000239804230613712,
-5.23358238829104));
#27232=CARTESIAN_POINT('Ctrl Pts',(-0.294541575596084,0.0164302863513783,
-5.2344600251021));
#27233=CARTESIAN_POINT('Ctrl Pts',(-0.293321228623321,0.0325992101967099,
-5.23533766191315));
#27234=CARTESIAN_POINT('Ctrl Pts',(-0.290661834729239,0.0485278758382486,
-5.23621529872421));
#27235=CARTESIAN_POINT('Ctrl Pts',(-0.274616462144716,0.144632997972109,
-5.24151049386571));
#27236=CARTESIAN_POINT('Ctrl Pts',(-0.206185814037005,0.231992059073534,
-5.24680568900721));
#27237=CARTESIAN_POINT('Ctrl Pts',(-0.116719156278496,0.270584359228645,
-5.25210088414871));
#27238=CARTESIAN_POINT('Ctrl Pts',(-0.0272524985199846,0.309176659383756,
-5.25739607929022));
#27239=CARTESIAN_POINT('Ctrl Pts',(0.0832501688893253,0.299002198592552,
-5.26269127443172));
#27240=CARTESIAN_POINT('Ctrl Pts',(0.164165658883164,0.244722073677462,
-5.26798646957322));
#27241=CARTESIAN_POINT('Ctrl Pts',(0.245081148877002,0.190441948762372,
-5.27328166471472));
#27242=CARTESIAN_POINT('Ctrl Pts',(0.296409461455368,0.0920561597233961,
-5.27857685985622));
#27243=CARTESIAN_POINT('Ctrl Pts',(0.294636207053114,-0.0053630583527391,
-5.28387205499773));
#27244=CARTESIAN_POINT('Ctrl Pts',(0.292862952650859,-0.102782276428872,
-5.28916725013923));
#27245=CARTESIAN_POINT('Ctrl Pts',(0.237988131267985,-0.199234923542167,
-5.29446244528074));
#27246=CARTESIAN_POINT('Ctrl Pts',(0.155150849617668,-0.250534370425409,
-5.29975764042224));
#27247=CARTESIAN_POINT('Ctrl Pts',(0.0723135679673499,-0.301833817308652,
-5.30505283556374));
#27248=CARTESIAN_POINT('Ctrl Pts',(-0.03848617395041,-0.307980063961841,
-5.31034803070524));
#27249=CARTESIAN_POINT('Ctrl Pts',(-0.126489094088413,-0.266157408272309,
-5.31564322584674));
#27250=CARTESIAN_POINT('Ctrl Pts',(-0.214492014226414,-0.224334752582778,
-5.32093842098825));
#27251=CARTESIAN_POINT('Ctrl Pts',(-0.279698112584657,-0.134543194550528,
-5.32623361612975));
#27252=CARTESIAN_POINT('Ctrl Pts',(-0.292235345415782,-0.0379178030911469,
-5.33152881127125));
#27253=CARTESIAN_POINT('Ctrl Pts',(-0.293856070906581,-0.0254267504716328,
-5.33221333694452));
#27254=CARTESIAN_POINT('Ctrl Pts',(-0.294596620428893,-0.0128214942159667,
-5.33289786261778));
#27255=CARTESIAN_POINT('Ctrl Pts',(-0.294496711936401,-0.000204427085817055,
-5.33358238829104));
#27256=CARTESIAN_POINT('Ctrl Pts',(-0.294542023011264,-0.000181426215594961,
-5.34801761170896));
#27257=CARTESIAN_POINT('Ctrl Pts',(-0.294620062553263,-0.0109624284817407,
-5.34743246395405));
#27258=CARTESIAN_POINT('Ctrl Pts',(-0.294079491686475,-0.021735523942461,
-5.34684731619914));
#27259=CARTESIAN_POINT('Ctrl Pts',(-0.292894307463314,-0.0324372302660748,
-5.34626216844423));
#27260=CARTESIAN_POINT('Ctrl Pts',(-0.282169184299795,-0.129280502508182,
-5.34096697330273));
#27261=CARTESIAN_POINT('Ctrl Pts',(-0.218656432482065,-0.220277691633531,
-5.33567177816123));
#27262=CARTESIAN_POINT('Ctrl Pts',(-0.131452344359818,-0.263741408227941,
-5.33037658301973));
#27263=CARTESIAN_POINT('Ctrl Pts',(-0.0442482562375699,-0.307205124822352,
-5.32508138787822));
#27264=CARTESIAN_POINT('Ctrl Pts',(0.0666471681891957,-0.30313536888582,
-5.31978619273672));
#27265=CARTESIAN_POINT('Ctrl Pts',(0.150430813057623,-0.253396566145975,
-5.31449099759522));
#27266=CARTESIAN_POINT('Ctrl Pts',(0.234214457926051,-0.20365776340613,
-5.30919580245371));
#27267=CARTESIAN_POINT('Ctrl Pts',(0.29088632323614,-0.108249913862972,
-5.30390060731221));
#27268=CARTESIAN_POINT('Ctrl Pts',(0.294484045307019,-0.0108810069094036,
-5.29860541217071));
#27269=CARTESIAN_POINT('Ctrl Pts',(0.298081767377898,0.0864879000441643,
-5.29331021702921));
#27270=CARTESIAN_POINT('Ctrl Pts',(0.248605346209566,0.185817864408143,
-5.28801502188771));
#27271=CARTESIAN_POINT('Ctrl Pts',(0.168720787817032,0.24160410801588,-5.28271982674621));
#27272=CARTESIAN_POINT('Ctrl Pts',(0.088836229424499,0.297390351623618,
-5.2774246316047));
#27273=CARTESIAN_POINT('Ctrl Pts',(-0.0214564661922352,0.309632874475115,
-5.2721294364632));
#27274=CARTESIAN_POINT('Ctrl Pts',(-0.111630303684109,0.272723164676459,
-5.2668342413217));
#27275=CARTESIAN_POINT('Ctrl Pts',(-0.201804141175983,0.235813454877802,
-5.26153904618019));
#27276=CARTESIAN_POINT('Ctrl Pts',(-0.271859120542995,0.149751512428991,
-5.25624385103869));
#27277=CARTESIAN_POINT('Ctrl Pts',(-0.289701841611522,0.0539638047087275,
-5.25094865589719));
#27278=CARTESIAN_POINT('Ctrl Pts',(-0.292993996259435,0.0362900459825212,
-5.24997164116778));
#27279=CARTESIAN_POINT('Ctrl Pts',(-0.294508646194196,0.0182851850559431,
-5.24899462643837));
#27280=CARTESIAN_POINT('Ctrl Pts',(-0.294344694043696,0.00025285010085293,
-5.24801761170896));
#27281=CARTESIAN_POINT('Origin',(0.,0.,-4.78));
#27282=CARTESIAN_POINT('',(-0.293729850984995,6.28784883607292E-5,-5.13358238829104));
#27283=CARTESIAN_POINT('',(-0.29372088508174,3.30216514158299E-5,-5.14801761170896));
#27284=CARTESIAN_POINT('',(-0.2942,-3.60291088309151E-17,-4.78));
#27285=CARTESIAN_POINT('Ctrl Pts',(-0.293729850984995,6.28784883607292E-5,
-5.13358238829104));
#27286=CARTESIAN_POINT('Ctrl Pts',(-0.29381626506198,0.0453324939186312,
-5.13602218758642));
#27287=CARTESIAN_POINT('Ctrl Pts',(-0.283993710042448,0.090566575165814,
-5.13846198688179));
#27288=CARTESIAN_POINT('Ctrl Pts',(-0.264067456747889,0.130796158920061,
-5.14090178617717));
#27289=CARTESIAN_POINT('Ctrl Pts',(-0.220820702871991,0.218108052502425,
-5.14619698131867));
#27290=CARTESIAN_POINT('Ctrl Pts',(-0.129981713533421,0.281846872486101,
-5.15149217646017));
#27291=CARTESIAN_POINT('Ctrl Pts',(-0.033165404082267,0.292812760776576,
-5.15678737160167));
#27292=CARTESIAN_POINT('Ctrl Pts',(0.0636509053688859,0.30377864906705,
-5.16208256674318));
#27293=CARTESIAN_POINT('Ctrl Pts',(0.166444534932621,0.261971605664325,
-5.16737776188468));
#27294=CARTESIAN_POINT('Ctrl Pts',(0.228123941385365,0.186544161710697,
-5.17267295702618));
#27295=CARTESIAN_POINT('Ctrl Pts',(0.289803347838111,0.111116717757068,
-5.17796815216768));
#27296=CARTESIAN_POINT('Ctrl Pts',(0.310368531179863,0.00206887325253695,
-5.18326334730918));
#27297=CARTESIAN_POINT('Ctrl Pts',(0.280398224505767,-0.090642664322898,
-5.18855854245068));
#27298=CARTESIAN_POINT('Ctrl Pts',(0.250427917831671,-0.183354201898333,
-5.19385373759219));
#27299=CARTESIAN_POINT('Ctrl Pts',(0.169922121141726,-0.259729432544673,
-5.19914893273369));
#27300=CARTESIAN_POINT('Ctrl Pts',(0.0757619351487175,-0.284779539440708,
-5.2044441278752));
#27301=CARTESIAN_POINT('Ctrl Pts',(-0.0183982508442894,-0.309829646336743,
-5.2097393230167));
#27302=CARTESIAN_POINT('Ctrl Pts',(-0.126212826140359,-0.283554629482476,
-5.2150345181582));
#27303=CARTESIAN_POINT('Ctrl Pts',(-0.198290065257727,-0.217991529472194,
-5.2203297132997));
#27304=CARTESIAN_POINT('Ctrl Pts',(-0.258421070742859,-0.163294995939315,
-5.22474727163015));
#27305=CARTESIAN_POINT('Ctrl Pts',(-0.293679382405638,-0.0812544975871136,
-5.2291648299606));
#27306=CARTESIAN_POINT('Ctrl Pts',(-0.294398673878215,0.000239804230613712,
-5.23358238829104));
#27307=CARTESIAN_POINT('Ctrl Pts',(-0.294344694043696,0.00025285010085293,
-5.24801761170896));
#27308=CARTESIAN_POINT('Ctrl Pts',(-0.293620063243877,-0.0794459233602251,
-5.24369943129687));
#27309=CARTESIAN_POINT('Ctrl Pts',(-0.260105003184177,-0.159681384578527,
-5.23938125088478));
#27310=CARTESIAN_POINT('Ctrl Pts',(-0.202338510586488,-0.214239063630774,
-5.23506307047268));
#27311=CARTESIAN_POINT('Ctrl Pts',(-0.131501995722885,-0.281140751258297,
-5.22976787533118));
#27312=CARTESIAN_POINT('Ctrl Pts',(-0.0241985032256398,-0.309430653521625,
-5.22447268018968));
#27313=CARTESIAN_POINT('Ctrl Pts',(0.0704143773112224,-0.286148675900522,
-5.21917748504818));
#27314=CARTESIAN_POINT('Ctrl Pts',(0.165027257848083,-0.262866698279419,
-5.21388228990667));
#27315=CARTESIAN_POINT('Ctrl Pts',(0.24694952642456,-0.188012840773886,
-5.20858709476517));
#27316=CARTESIAN_POINT('Ctrl Pts',(0.278651172007717,-0.0958789528023486,
-5.20329189962367));
#27317=CARTESIAN_POINT('Ctrl Pts',(0.310352817590874,-0.00374506483081084,
-5.19799670448217));
#27318=CARTESIAN_POINT('Ctrl Pts',(0.291833840180711,0.10566885360673,-5.19270150934067));
#27319=CARTESIAN_POINT('Ctrl Pts',(0.231578104281948,0.182238390217124,
-5.18740631419916));
#27320=CARTESIAN_POINT('Ctrl Pts',(0.171322368383185,0.258807926827517,
-5.18211111905766));
#27321=CARTESIAN_POINT('Ctrl Pts',(0.0693298739958214,0.302533081610763,
-5.17681592391616));
#27322=CARTESIAN_POINT('Ctrl Pts',(-0.0276748495653676,0.293382603358283,
-5.17152072877465));
#27323=CARTESIAN_POINT('Ctrl Pts',(-0.124679573126557,0.284232125105803,
-5.16622553363315));
#27324=CARTESIAN_POINT('Ctrl Pts',(-0.216696525861573,0.222206013817596,
-5.16093033849165));
#27325=CARTESIAN_POINT('Ctrl Pts',(-0.261571146973085,0.13571950605176,
-5.15563514335015));
#27326=CARTESIAN_POINT('Ctrl Pts',(-0.283089639182754,0.0942470836111143,
-5.15309596613642));
#27327=CARTESIAN_POINT('Ctrl Pts',(-0.293768035010674,0.0471501397218707,
-5.15055678892269));
#27328=CARTESIAN_POINT('Ctrl Pts',(-0.29372088508174,3.30216514158299E-5,
-5.14801761170896));
#27329=CARTESIAN_POINT('Origin',(0.,0.,-4.78));
#27330=CARTESIAN_POINT('',(-0.294167685007082,-0.000269782114602712,-5.03358238829104));
#27331=CARTESIAN_POINT('',(-0.294223320968512,-0.000268522322062943,-5.04801761170896));
#27332=CARTESIAN_POINT('',(-0.2942,-3.60291088309151E-17,-4.78));
#27333=CARTESIAN_POINT('Ctrl Pts',(-0.294167685007082,-0.000269782114602712,
-5.03358238829104));
#27334=CARTESIAN_POINT('Ctrl Pts',(-0.2934934036862,0.0737067916099429,
-5.03758435007074));
#27335=CARTESIAN_POINT('Ctrl Pts',(-0.265170690824886,0.148143361035309,
-5.04158631185043));
#27336=CARTESIAN_POINT('Ctrl Pts',(-0.214741519260896,0.20180519519344,
-5.04558827363013));
#27337=CARTESIAN_POINT('Ctrl Pts',(-0.148016168306652,0.272807843184718,
-5.05088346877163));
#27338=CARTESIAN_POINT('Ctrl Pts',(-0.042588475632073,0.307439631678508,
-5.05617866391313));
#27339=CARTESIAN_POINT('Ctrl Pts',(0.0532433055771352,0.289835138160921,
-5.06147385905463));
#27340=CARTESIAN_POINT('Ctrl Pts',(0.149075086786345,0.272230644643333,
-5.06676905419613));
#27341=CARTESIAN_POINT('Ctrl Pts',(0.235310956530186,0.202389869114365,
-5.07206424933764));
#27342=CARTESIAN_POINT('Ctrl Pts',(0.272444768321761,0.112308081257059,
-5.07735944447914));
#27343=CARTESIAN_POINT('Ctrl Pts',(0.309578580113335,0.0222262933997549,
-5.08265463962064));
#27344=CARTESIAN_POINT('Ctrl Pts',(0.297610333952645,-0.0880965067858862,
-5.08794983476214));
#27345=CARTESIAN_POINT('Ctrl Pts',(0.242022890828046,-0.168119532526044,
-5.09324502990365));
#27346=CARTESIAN_POINT('Ctrl Pts',(0.186435447703447,-0.248142558266203,
-5.09854022504515));
#27347=CARTESIAN_POINT('Ctrl Pts',(0.0872288076149375,-0.297865809560878,
-5.10383542018665));
#27348=CARTESIAN_POINT('Ctrl Pts',(-0.010148748258762,-0.294510203236357,
-5.10913061532816));
#27349=CARTESIAN_POINT('Ctrl Pts',(-0.107526304132462,-0.291154596911837,
-5.11442581046966));
#27350=CARTESIAN_POINT('Ctrl Pts',(-0.203074775791352,-0.234720132968122,
-5.11972100561116));
#27351=CARTESIAN_POINT('Ctrl Pts',(-0.253021752414184,-0.151060417405737,
-5.12501620075266));
#27352=CARTESIAN_POINT('Ctrl Pts',(-0.279955299859418,-0.105947518273335,
-5.12787159659879));
#27353=CARTESIAN_POINT('Ctrl Pts',(-0.293628717093803,-0.0529179843639099,
-5.13072699244491));
#27354=CARTESIAN_POINT('Ctrl Pts',(-0.293729850984995,6.28784883607292E-5,
-5.13358238829104));
#27355=CARTESIAN_POINT('Ctrl Pts',(-0.29372088508174,3.30216514158299E-5,
-5.14801761170896));
#27356=CARTESIAN_POINT('Ctrl Pts',(-0.293669708642092,-0.0511078051506823,
-5.14526159378119));
#27357=CARTESIAN_POINT('Ctrl Pts',(-0.280982886140013,-0.102272398931093,
-5.14250557585341));
#27358=CARTESIAN_POINT('Ctrl Pts',(-0.255806892924437,-0.146294507019556,
-5.13974955792564));
#27359=CARTESIAN_POINT('Ctrl Pts',(-0.207435728276266,-0.23087510808157,
-5.13445436278414));
#27360=CARTESIAN_POINT('Ctrl Pts',(-0.112961109491914,-0.28908940596213,
-5.12915916764264));
#27361=CARTESIAN_POINT('Ctrl Pts',(-0.0156634967798184,-0.294268421887871,
-5.12386397250114));
#27362=CARTESIAN_POINT('Ctrl Pts',(0.0816341159322764,-0.299447437813612,
-5.11856877735963));
#27363=CARTESIAN_POINT('Ctrl Pts',(0.181754722572115,-0.251591171784534,
-5.11327358221813));
#27364=CARTESIAN_POINT('Ctrl Pts',(0.238831338043824,-0.172623408667382,
-5.10797838707663));
#27365=CARTESIAN_POINT('Ctrl Pts',(0.295907953515533,-0.0936556455502302,
-5.10268319193513));
#27366=CARTESIAN_POINT('Ctrl Pts',(0.309940577819113,0.0164236146549957,
-5.09738799679363));
#27367=CARTESIAN_POINT('Ctrl Pts',(0.27450062256113,0.107185155060303,-5.09209280165212));
#27368=CARTESIAN_POINT('Ctrl Pts',(0.239060667303148,0.197946695465609,
-5.08679760651062));
#27369=CARTESIAN_POINT('Ctrl Pts',(0.154148132483604,0.269390516070998,
-5.08150241136912));
#27370=CARTESIAN_POINT('Ctrl Pts',(0.0586629219258051,0.28878696446148,
-5.07620721622761));
#27371=CARTESIAN_POINT('Ctrl Pts',(-0.0368222886319945,0.308183412851963,
-5.07091202108611));
#27372=CARTESIAN_POINT('Ctrl Pts',(-0.14288017492805,0.275532489027539,
-5.06561682594461));
#27373=CARTESIAN_POINT('Ctrl Pts',(-0.210923781156748,0.20579214706662,
-5.06032163080311));
#27374=CARTESIAN_POINT('Ctrl Pts',(-0.26362626632805,0.151775472440597,
-5.05622029110506));
#27375=CARTESIAN_POINT('Ctrl Pts',(-0.293523528977382,0.0755084110569016,
-5.05211895140701));
#27376=CARTESIAN_POINT('Ctrl Pts',(-0.294223320968512,-0.000268522322062943,
-5.04801761170896));
#27377=CARTESIAN_POINT('Origin',(0.,0.,-4.78));
#27378=CARTESIAN_POINT('',(-0.294651137856664,9.05457447918836E-5,-4.93358238829104));
#27379=CARTESIAN_POINT('',(-0.294623644711037,0.000121576380800716,-4.94801761170896));
#27380=CARTESIAN_POINT('',(-0.2942,-3.60291088309151E-17,-4.78));
#27381=CARTESIAN_POINT('Ctrl Pts',(-0.294651137856664,9.05457447918836E-5,
-4.93358238829104));
#27382=CARTESIAN_POINT('Ctrl Pts',(-0.294671139319386,0.00504055750254152,
-4.93385131741355));
#27383=CARTESIAN_POINT('Ctrl Pts',(-0.294557213003961,0.00998962927470263,
-4.93412024653607));
#27384=CARTESIAN_POINT('Ctrl Pts',(-0.294306471987783,0.0149317596968457,
-4.93438917565858));
#27385=CARTESIAN_POINT('Ctrl Pts',(-0.289369399356023,0.112241953384708,
-4.93968437080008));
#27386=CARTESIAN_POINT('Ctrl Pts',(-0.231390187092484,0.206861032339553,
-4.94497956594158));
#27387=CARTESIAN_POINT('Ctrl Pts',(-0.146930117175096,0.255442356645199,
-4.95027476108308));
#27388=CARTESIAN_POINT('Ctrl Pts',(-0.0624700472577058,0.304023680950845,
-4.95556995622458));
#27389=CARTESIAN_POINT('Ctrl Pts',(0.048470880313534,0.306567250607288,
-4.96086515136609));
#27390=CARTESIAN_POINT('Ctrl Pts',(0.13506870389667,0.261907812272208,-4.96616034650759));
#27391=CARTESIAN_POINT('Ctrl Pts',(0.221666527479803,0.217248373937128,
-4.9714555416491));
#27392=CARTESIAN_POINT('Ctrl Pts',(0.283921247074832,0.125385927610527,
-4.9767507367906));
#27393=CARTESIAN_POINT('Ctrl Pts',(0.293312896696289,0.028404252026281,
-4.9820459319321));
#27394=CARTESIAN_POINT('Ctrl Pts',(0.302704546317745,-0.0685774235579688,
-4.9873411270736));
#27395=CARTESIAN_POINT('Ctrl Pts',(0.259233125965623,-0.170678328399865,
-4.99263632221511));
#27396=CARTESIAN_POINT('Ctrl Pts',(0.182813646708123,-0.231124268476544,
-4.99793151735661));
#27397=CARTESIAN_POINT('Ctrl Pts',(0.106394167450625,-0.291570208553221,
-5.00322671249811));
#27398=CARTESIAN_POINT('Ctrl Pts',(-0.00297337071224937,-0.310361183864684,
-5.00852190763961));
#27399=CARTESIAN_POINT('Ctrl Pts',(-0.095185803094993,-0.278888722953621,
-5.01381710278111));
#27400=CARTESIAN_POINT('Ctrl Pts',(-0.187398235477738,-0.247416262042557,
-5.01911229792261));
#27401=CARTESIAN_POINT('Ctrl Pts',(-0.262455562080351,-0.165680364908966,
-5.02440749306412));
#27402=CARTESIAN_POINT('Ctrl Pts',(-0.285972720764702,-0.0711256625977863,
-5.02970268820562));
#27403=CARTESIAN_POINT('Ctrl Pts',(-0.291716262479935,-0.0480327845683877,
-5.03099592156743));
#27404=CARTESIAN_POINT('Ctrl Pts',(-0.294385578916972,-0.0241753010573829,
-5.03228915492924));
#27405=CARTESIAN_POINT('Ctrl Pts',(-0.294167685007082,-0.000269782114602712,
-5.03358238829104));
#27406=CARTESIAN_POINT('Ctrl Pts',(-0.294223320968512,-0.000268522322062943,
-5.04801761170896));
#27407=CARTESIAN_POINT('Ctrl Pts',(-0.29442702281703,-0.0223263646523878,
-5.04682375626551));
#27408=CARTESIAN_POINT('Ctrl Pts',(-0.292156738679848,-0.0443426770218096,
-5.04562990082206));
#27409=CARTESIAN_POINT('Ctrl Pts',(-0.28725480488683,-0.0657565686542278,
-5.0444360453786));
#27410=CARTESIAN_POINT('Ctrl Pts',(-0.265512896226875,-0.160735182316747,
-5.0391408502371));
#27411=CARTESIAN_POINT('Ctrl Pts',(-0.191999752745621,-0.243862649544373,
-5.0338456550956));
#27412=CARTESIAN_POINT('Ctrl Pts',(-0.100393019531007,-0.277056836914731,
-5.02855045995409));
#27413=CARTESIAN_POINT('Ctrl Pts',(-0.00878628631639407,-0.31025102428509,
-5.02325526481259));
#27414=CARTESIAN_POINT('Ctrl Pts',(0.10091403663158,-0.293511931798183,
-5.01796006967109));
#27415=CARTESIAN_POINT('Ctrl Pts',(0.178452330149845,-0.234508027828132,
-5.01266487452959));
#27416=CARTESIAN_POINT('Ctrl Pts',(0.255990623668112,-0.17550412385808,
-5.00736967938809));
#27417=CARTESIAN_POINT('Ctrl Pts',(0.30136688775667,-0.0742354084048829,
-5.00207448424658));
#27418=CARTESIAN_POINT('Ctrl Pts',(0.293793469418738,0.0229051648902689,
-4.99677928910508));
#27419=CARTESIAN_POINT('Ctrl Pts',(0.286220051080805,0.12004573818542,-4.99148409396357));
#27420=CARTESIAN_POINT('Ctrl Pts',(0.225696950316382,0.213058169322525,
-4.98618889882207));
#27421=CARTESIAN_POINT('Ctrl Pts',(0.139950848513885,0.259331851595582,
-4.98089370368057));
#27422=CARTESIAN_POINT('Ctrl Pts',(0.0542047467113887,0.305605533868638,
-4.97559850853907));
#27423=CARTESIAN_POINT('Ctrl Pts',(-0.0567643561291807,0.305140467277647,
-4.97030331339757));
#27424=CARTESIAN_POINT('Ctrl Pts',(-0.142119590786683,0.258149706888029,
-4.96500811825607));
#27425=CARTESIAN_POINT('Ctrl Pts',(-0.227474825444186,0.21115894649841,
-4.95971292311456));
#27426=CARTESIAN_POINT('Ctrl Pts',(-0.287216191918622,0.117642492310163,
-4.95441772797306));
#27427=CARTESIAN_POINT('Ctrl Pts',(-0.293975134848083,0.0204418527242618,
-4.94912253283156));
#27428=CARTESIAN_POINT('Ctrl Pts',(-0.294445252795243,0.0136810669591461,
-4.94875422579069));
#27429=CARTESIAN_POINT('Ctrl Pts',(-0.294659047538173,0.00690245750566513,
-4.94838591874983));
#27430=CARTESIAN_POINT('Ctrl Pts',(-0.294623644711037,0.000121576380800716,
-4.94801761170896));
#27431=CARTESIAN_POINT('Origin',(0.,0.,-4.78));
#27432=CARTESIAN_POINT('',(-0.293898321762298,0.000215997425517533,-4.83358238829104));
#27433=CARTESIAN_POINT('',(-0.293858731285566,0.00019623248150203,-4.84801761170896));
#27434=CARTESIAN_POINT('',(-0.2942,-3.60291088309151E-17,-4.78));
#27435=CARTESIAN_POINT('Ctrl Pts',(-0.293898321762298,0.000215997425517533,
-4.83358238829104));
#27436=CARTESIAN_POINT('Ctrl Pts',(-0.29412892854093,0.0341424934738597,
-4.83541347989787));
#27437=CARTESIAN_POINT('Ctrl Pts',(-0.288705448149838,0.0679975401570607,
-4.8372445715047));
#27438=CARTESIAN_POINT('Ctrl Pts',(-0.277305616806589,0.0997038203333129,
-4.83907566311153));
#27439=CARTESIAN_POINT('Ctrl Pts',(-0.244339307902389,0.191392810724597,
-4.84437085825304));
#27440=CARTESIAN_POINT('Ctrl Pts',(-0.161394882146101,0.265112424077647,
-4.84966605339454));
#27441=CARTESIAN_POINT('Ctrl Pts',(-0.0664706184897772,0.287090427877919,
-4.85496124853604));
#27442=CARTESIAN_POINT('Ctrl Pts',(0.0284536451665497,0.309068431678192,
-4.86025644367755));
#27443=CARTESIAN_POINT('Ctrl Pts',(0.135357746722915,0.279304825925683,
-4.86555163881905));
#27444=CARTESIAN_POINT('Ctrl Pts',(0.205267064497167,0.211434834249837,
-4.87084683396055));
#27445=CARTESIAN_POINT('Ctrl Pts',(0.275176382271419,0.143564842573991,
-4.87614202910205));
#27446=CARTESIAN_POINT('Ctrl Pts',(0.308090916263558,0.0375884649748095,
-4.88143722424355));
#27447=CARTESIAN_POINT('Ctrl Pts',(0.288931948008704,-0.0579446832887666,
-4.88673241938505));
#27448=CARTESIAN_POINT('Ctrl Pts',(0.269772979753852,-0.15347783155234,
-4.89202761452656));
#27449=CARTESIAN_POINT('Ctrl Pts',(0.198540509252008,-0.238567750480307,
-4.89732280966807));
#27450=CARTESIAN_POINT('Ctrl Pts',(0.107867365772809,-0.274233273515041,
-4.90261800480957));
#27451=CARTESIAN_POINT('Ctrl Pts',(0.01719422229361,-0.309898796549775,
-4.90791319995107));
#27452=CARTESIAN_POINT('Ctrl Pts',(-0.0929195941629457,-0.296139923691275,
-4.91320839509257));
#27453=CARTESIAN_POINT('Ctrl Pts',(-0.172029035891234,-0.239259833051586,
-4.91850359023407));
#27454=CARTESIAN_POINT('Ctrl Pts',(-0.247120715822662,-0.18526853356225,
-4.92352985625306));
#27455=CARTESIAN_POINT('Ctrl Pts',(-0.294277311952389,-0.0924248191183649,
-4.92855612227205));
#27456=CARTESIAN_POINT('Ctrl Pts',(-0.294651137856664,9.05457447918836E-5,
-4.93358238829104));
#27457=CARTESIAN_POINT('Ctrl Pts',(-0.294623644711037,0.000121576380800716,
-4.94801761170896));
#27458=CARTESIAN_POINT('Ctrl Pts',(-0.29415005678468,-0.0905870955125116,
-4.94309072360833));
#27459=CARTESIAN_POINT('Ctrl Pts',(-0.249083215497219,-0.181702277058098,
-4.93816383550769));
#27460=CARTESIAN_POINT('Ctrl Pts',(-0.176480470572474,-0.235995535462575,
-4.93323694740705));
#27461=CARTESIAN_POINT('Ctrl Pts',(-0.0984503439829113,-0.294347459079958,
-4.92794175226555));
#27462=CARTESIAN_POINT('Ctrl Pts',(0.0113864285807017,-0.310166481331168,
-4.92264655712404));
#27463=CARTESIAN_POINT('Ctrl Pts',(0.10271171802156,-0.27620563396283,-4.91735136198254));
#27464=CARTESIAN_POINT('Ctrl Pts',(0.194037007462415,-0.242244786594493,
-4.91205616684104));
#27465=CARTESIAN_POINT('Ctrl Pts',(0.266850813780515,-0.158504069606611,
-4.90676097169955));
#27466=CARTESIAN_POINT('Ctrl Pts',(0.287795870362606,-0.0633465567649832,
-4.90146577655804));
#27467=CARTESIAN_POINT('Ctrl Pts',(0.308740926944698,0.0318109560766487,
-4.89617058141654));
#27468=CARTESIAN_POINT('Ctrl Pts',(0.277817233790773,0.13838526477203,-4.89087538627503));
#27469=CARTESIAN_POINT('Ctrl Pts',(0.209191470674386,0.207552831464273,
-4.88558019113353));
#27470=CARTESIAN_POINT('Ctrl Pts',(0.140565707558001,0.276720398156514,
-4.88028499599203));
#27471=CARTESIAN_POINT('Ctrl Pts',(0.0342378744791568,0.308481222845622,
-4.87498980085053));
#27472=CARTESIAN_POINT('Ctrl Pts',(-0.0610814054568818,0.288285121293419,
-4.86969460570903));
#27473=CARTESIAN_POINT('Ctrl Pts',(-0.15640068539292,0.268089019741216,
-4.86439941056753));
#27474=CARTESIAN_POINT('Ctrl Pts',(-0.240711412186152,0.195935991947701,
-4.85910421542602));
#27475=CARTESIAN_POINT('Ctrl Pts',(-0.275389380700085,0.104880590432038,
-4.85380902028452));
#27476=CARTESIAN_POINT('Ctrl Pts',(-0.288031929203502,0.0716845187043262,
-4.85187855075933));
#27477=CARTESIAN_POINT('Ctrl Pts',(-0.294077722442252,0.0359761075925212,
-4.84994808123415));
#27478=CARTESIAN_POINT('Ctrl Pts',(-0.293858731285566,0.00019623248150203,
-4.84801761170896));
#27479=CARTESIAN_POINT('Origin',(0.,0.,-4.78));
#27480=CARTESIAN_POINT('',(-0.293869683561436,-0.000202171647430832,-4.73358238829104));
#27481=CARTESIAN_POINT('',(-0.29391040772598,-0.000221175939017525,-4.74801761170896));
#27482=CARTESIAN_POINT('',(-0.2942,-3.60291088309151E-17,-4.78));
#27483=CARTESIAN_POINT('Ctrl Pts',(-0.293869683561436,-0.000202171647430832,
-4.73358238829104));
#27484=CARTESIAN_POINT('Ctrl Pts',(-0.293472176975345,0.0626834963700132,
-4.73697564238219));
#27485=CARTESIAN_POINT('Ctrl Pts',(-0.273702122510387,0.125797236938147,
-4.74036889647334));
#27486=CARTESIAN_POINT('Ctrl Pts',(-0.236433629577098,0.175893137178628,
-4.7437621505645));
#27487=CARTESIAN_POINT('Ctrl Pts',(-0.178275903273585,0.254068116250875,
-4.749057345706));
#27488=CARTESIAN_POINT('Ctrl Pts',(-0.0775063189671733,0.300542303018127,
-4.7543525408475));
#27489=CARTESIAN_POINT('Ctrl Pts',(0.0197108303297479,0.29402506707635,
-4.759647735989));
#27490=CARTESIAN_POINT('Ctrl Pts',(0.11692797962667,0.287507831134573,-4.7649429311305));
#27491=CARTESIAN_POINT('Ctrl Pts',(0.210592693914104,0.227999172483765,
-4.77023812627201));
#27492=CARTESIAN_POINT('Ctrl Pts',(0.257795544270133,0.142761038998762,
-4.77553332141351));
#27493=CARTESIAN_POINT('Ctrl Pts',(0.304998394626161,0.0575229055137613,
-4.78082851655501));
#27494=CARTESIAN_POINT('Ctrl Pts',(0.305739381050789,-0.0534447028054307,
-4.78612371169651));
#27495=CARTESIAN_POINT('Ctrl Pts',(0.259679044820831,-0.139305601403824,
-4.79141890683801));
#27496=CARTESIAN_POINT('Ctrl Pts',(0.213618708590872,-0.225166500002218,
-4.79671410197952));
#27497=CARTESIAN_POINT('Ctrl Pts',(0.120757049706323,-0.28592068887981,
-4.80200929712102));
#27498=CARTESIAN_POINT('Ctrl Pts',(0.0236356034912526,-0.293735621178543,
-4.80730449226252));
#27499=CARTESIAN_POINT('Ctrl Pts',(-0.0734858427238168,-0.301550553477275,
-4.81259968740402));
#27500=CARTESIAN_POINT('Ctrl Pts',(-0.17486707626941,-0.25642622919715,
-4.81789488254553));
#27501=CARTESIAN_POINT('Ctrl Pts',(-0.234063597016152,-0.179034883342326,
-4.82319007768703));
#27502=CARTESIAN_POINT('Ctrl Pts',(-0.272789814139247,-0.128405656738881,
-4.8266541812217));
#27503=CARTESIAN_POINT('Ctrl Pts',(-0.293462054262629,-0.0639669710516069,
-4.83011828475637));
#27504=CARTESIAN_POINT('Ctrl Pts',(-0.293898321762298,0.000215997425517533,
-4.83358238829104));
#27505=CARTESIAN_POINT('Ctrl Pts',(-0.293858731285566,0.00019623248150203,
-4.84801761170896));
#27506=CARTESIAN_POINT('Ctrl Pts',(-0.29347703908839,-0.0621665558267297,
-4.84465288609264));
#27507=CARTESIAN_POINT('Ctrl Pts',(-0.27406356122904,-0.124746444585632,
-4.84128816047633));
#27508=CARTESIAN_POINT('Ctrl Pts',(-0.237376059777544,-0.174619172762435,
-4.83792343486001));
#27509=CARTESIAN_POINT('Ctrl Pts',(-0.179639560106439,-0.253105759203433,
-4.83262823971851));
#27510=CARTESIAN_POINT('Ctrl Pts',(-0.079121350529597,-0.30012115684762,
-4.82733304457701));
#27511=CARTESIAN_POINT('Ctrl Pts',(0.0181294350607954,-0.294126797208492,
-4.82203784943551));
#27512=CARTESIAN_POINT('Ctrl Pts',(0.115380220651189,-0.288132437569365,
-4.816742654294));
#27513=CARTESIAN_POINT('Ctrl Pts',(0.209363582255135,-0.229128320646921,
-4.8114474591525));
#27514=CARTESIAN_POINT('Ctrl Pts',(0.257024113092535,-0.144145255006,-4.806152264011));
#27515=CARTESIAN_POINT('Ctrl Pts',(0.304684643929936,-0.0591621893650789,
-4.80085706886949));
#27516=CARTESIAN_POINT('Ctrl Pts',(0.306022344000792,0.0517998249943176,
-4.795561873728));
#27517=CARTESIAN_POINT('Ctrl Pts',(0.260424389718913,0.13790716620713,-4.79026667858649));
#27518=CARTESIAN_POINT('Ctrl Pts',(0.214826435437034,0.224014507419941,
-4.78497148344499));
#27519=CARTESIAN_POINT('Ctrl Pts',(0.122292826802418,0.285267175486166,
-4.77967628830348));
#27520=CARTESIAN_POINT('Ctrl Pts',(0.0252148136341864,0.29360426159227,
-4.77438109316198));
#27521=CARTESIAN_POINT('Ctrl Pts',(-0.0718631995340452,0.301941347698375,
-4.76908589802048));
#27522=CARTESIAN_POINT('Ctrl Pts',(-0.173485617235893,0.25736285184436,
-4.76379070287898));
#27523=CARTESIAN_POINT('Ctrl Pts',(-0.233097448700031,0.180290955572612,
-4.75849550773748));
#27524=CARTESIAN_POINT('Ctrl Pts',(-0.272416526685478,0.129455478360035,
-4.75500287572798));
#27525=CARTESIAN_POINT('Ctrl Pts',(-0.293458791912228,0.0644836643687234,
-4.75151024371847));
#27526=CARTESIAN_POINT('Ctrl Pts',(-0.29391040772598,-0.000221175939017525,
-4.74801761170896));
#27527=CARTESIAN_POINT('Origin',(0.,0.,-4.78));
#27528=CARTESIAN_POINT('',(-0.294632262618422,-0.000112863968801113,-4.63358238829104));
#27529=CARTESIAN_POINT('',(-0.294657663022813,-8.13145974722069E-5,-4.64801761170896));
#27530=CARTESIAN_POINT('',(-0.2942,-3.60291088309151E-17,-4.78));
#27531=CARTESIAN_POINT('Ctrl Pts',(-0.294632262618422,-0.000112863968801113,
-4.63358238829104));
#27532=CARTESIAN_POINT('Ctrl Pts',(-0.294185344683986,0.0911139735210852,
-4.63853780486651));
#27533=CARTESIAN_POINT('Ctrl Pts',(-0.248524608202355,0.182726981672203,
-4.64349322144198));
#27534=CARTESIAN_POINT('Ctrl Pts',(-0.175208868908362,0.236941151253623,
-4.64844863801746));
#27535=CARTESIAN_POINT('Ctrl Pts',(-0.0968660816587778,0.29487262946458,
-4.65374383315896));
#27536=CARTESIAN_POINT('Ctrl Pts',(0.0130541738897331,0.310100780275279,
-4.65903902830046));
#27537=CARTESIAN_POINT('Ctrl Pts',(0.104195523638138,0.275649323879661,
-4.66433422344196));
#27538=CARTESIAN_POINT('Ctrl Pts',(0.195336873386545,0.241197867484043,
-4.66962941858346));
#27539=CARTESIAN_POINT('Ctrl Pts',(0.267699317334844,0.157066803882104,
-4.67492461372497));
#27540=CARTESIAN_POINT('Ctrl Pts',(0.288132365793964,0.0617980313886571,
-4.68021980886647));
#27541=CARTESIAN_POINT('Ctrl Pts',(0.308565414253084,-0.0334707411047907,
-4.68551500400797));
#27542=CARTESIAN_POINT('Ctrl Pts',(0.277069067223022,-0.139877222489745,
-4.69081019914947));
#27543=CARTESIAN_POINT('Ctrl Pts',(0.208072347142677,-0.208674759508852,
-4.69610539429097));
#27544=CARTESIAN_POINT('Ctrl Pts',(0.139075627062335,-0.277472296527957,
-4.70140058943247));
#27545=CARTESIAN_POINT('Ctrl Pts',(0.0325785339317089,-0.308660889181219,
-4.70669578457398));
#27546=CARTESIAN_POINT('Ctrl Pts',(-0.0626307681807567,-0.287952502643454,
-4.71199097971548));
#27547=CARTESIAN_POINT('Ctrl Pts',(-0.157840070293225,-0.267244116105689,
-4.71728617485699));
#27548=CARTESIAN_POINT('Ctrl Pts',(-0.241761581387535,-0.194638750376895,
-4.72258136999848));
#27549=CARTESIAN_POINT('Ctrl Pts',(-0.275949402784381,-0.103398181823877,
-4.72787656513999));
#27550=CARTESIAN_POINT('Ctrl Pts',(-0.288229067499113,-0.0706261728325144,
-4.72977850619034));
#27551=CARTESIAN_POINT('Ctrl Pts',(-0.294092488595649,-0.0354499987385414,
-4.73168044724069));
#27552=CARTESIAN_POINT('Ctrl Pts',(-0.293869683561436,-0.000202171647430832,
-4.73358238829104));
#27553=CARTESIAN_POINT('Ctrl Pts',(-0.29391040772598,-0.000221175939017525,
-4.74801761170896));
#27554=CARTESIAN_POINT('Ctrl Pts',(-0.294143488684261,-0.0336156358429093,
-4.74621504857697));
#27555=CARTESIAN_POINT('Ctrl Pts',(-0.28889196467631,-0.0669389836045177,
-4.74441248544497));
#27556=CARTESIAN_POINT('Ctrl Pts',(-0.277837748893218,-0.0982111732019241,
-4.74260992231297));
#27557=CARTESIAN_POINT('Ctrl Pts',(-0.245364972395839,-0.190076109015233,
-4.73731472717147));
#27558=CARTESIAN_POINT('Ctrl Pts',(-0.162818174174651,-0.264240683952366,
-4.73201953202996));
#27559=CARTESIAN_POINT('Ctrl Pts',(-0.0680134731165798,-0.286728820885466,
-4.72672433688846));
#27560=CARTESIAN_POINT('Ctrl Pts',(0.02679122794149,-0.309216957818565,
-4.72142914174696));
#27561=CARTESIAN_POINT('Ctrl Pts',(0.133853831836441,-0.280028656747631,
-4.71613394660546));
#27562=CARTESIAN_POINT('Ctrl Pts',(0.20412710421781,-0.21253558425685,-4.71083875146396));
#27563=CARTESIAN_POINT('Ctrl Pts',(0.274400376599178,-0.145042511766069,
-4.70554355632246));
#27564=CARTESIAN_POINT('Ctrl Pts',(0.307884317466962,-0.0392446678554377,
-4.70024836118095));
#27565=CARTESIAN_POINT('Ctrl Pts',(0.289239353198137,0.0563901215929949,
-4.69495316603945));
#27566=CARTESIAN_POINT('Ctrl Pts',(0.27059438892931,0.15202491104143,-4.68965797089795));
#27567=CARTESIAN_POINT('Ctrl Pts',(0.199820519523876,0.237496646027665,
-4.68436277575645));
#27568=CARTESIAN_POINT('Ctrl Pts',(0.109340481141167,0.273649243440517,
-4.67906758061494));
#27569=CARTESIAN_POINT('Ctrl Pts',(0.0188604427584614,0.309801840853368,
-4.67377238547344));
#27570=CARTESIAN_POINT('Ctrl Pts',(-0.0913257646015185,0.296635300692835,
-4.66847719033194));
#27571=CARTESIAN_POINT('Ctrl Pts',(-0.170739929705677,0.240181443196284,
-4.66318199519044));
#27572=CARTESIAN_POINT('Ctrl Pts',(-0.246548709887166,0.186290577911231,
-4.65812720069661));
#27573=CARTESIAN_POINT('Ctrl Pts',(-0.29431610970276,0.0929536427050627,
-4.65307240620278));
#27574=CARTESIAN_POINT('Ctrl Pts',(-0.294657663022813,-8.13145974722069E-5,
-4.64801761170896));
#27575=CARTESIAN_POINT('Origin',(0.,0.,-4.78));
#27576=CARTESIAN_POINT('',(-0.294207300827486,0.000269263671129533,-4.53358238829104));
#27577=CARTESIAN_POINT('',(-0.294151842938781,0.000269461638096479,-4.54801761170896));
#27578=CARTESIAN_POINT('',(-0.2942,-3.60291088309151E-17,-4.78));
#27579=CARTESIAN_POINT('Ctrl Pts',(-0.294207300827486,0.000269263671129533,
-4.53358238829104));
#27580=CARTESIAN_POINT('Ctrl Pts',(-0.294415377118081,0.0228573529575127,
-4.53480477220933));
#27581=CARTESIAN_POINT('Ctrl Pts',(-0.29203396319701,0.0454020295514724,
-4.53602715612762));
#27582=CARTESIAN_POINT('Ctrl Pts',(-0.286897060561383,0.0673003234968311,
-4.5372495400459));
#27583=CARTESIAN_POINT('Ctrl Pts',(-0.264644721119102,0.162160651722523,
-4.54254473518741));
#27584=CARTESIAN_POINT('Ctrl Pts',(-0.190685622245191,0.244891606332771,
-4.54783993032891));
#27585=CARTESIAN_POINT('Ctrl Pts',(-0.0989017089218338,0.277592703207201,
-4.55313512547041));
#27586=CARTESIAN_POINT('Ctrl Pts',(-0.00711779559847499,0.310293800081631,
-4.55843032061192));
#27587=CARTESIAN_POINT('Ctrl Pts',(0.102490932174331,0.292965039220241,
-4.56372551575342));
#27588=CARTESIAN_POINT('Ctrl Pts',(0.179710816570699,0.233545026299069,
-4.56902071089492));
#27589=CARTESIAN_POINT('Ctrl Pts',(0.256930700967065,0.174125013377898,
-4.57431590603642));
#27590=CARTESIAN_POINT('Ctrl Pts',(0.301761741986994,0.0726137483969471,
-4.57961110117793));
#27591=CARTESIAN_POINT('Ctrl Pts',(0.293666062770727,-0.0244846988602953,
-4.58490629631943));
#27592=CARTESIAN_POINT('Ctrl Pts',(0.285570383554461,-0.12158314611754,
-4.59020149146093));
#27593=CARTESIAN_POINT('Ctrl Pts',(0.224547984101994,-0.214268775651076,
-4.59549668660243));
#27594=CARTESIAN_POINT('Ctrl Pts',(0.138554283184103,-0.260080694233308,
-4.60079188174393));
#27595=CARTESIAN_POINT('Ctrl Pts',(0.0525605822662109,-0.30589261281554,
-4.60608707688543));
#27596=CARTESIAN_POINT('Ctrl Pts',(-0.0584044201171068,-0.304830820446466,
-4.61138227202694));
#27597=CARTESIAN_POINT('Ctrl Pts',(-0.14350573323524,-0.257381742612324,
-4.61667746716844));
#27598=CARTESIAN_POINT('Ctrl Pts',(-0.22860704635337,-0.209932664778183,
-4.62197266230994));
#27599=CARTESIAN_POINT('Ctrl Pts',(-0.287844670206317,-0.116096301478976,
-4.62726785745144));
#27600=CARTESIAN_POINT('Ctrl Pts',(-0.294080822657462,-0.0188607170237647,
-4.63256305259294));
#27601=CARTESIAN_POINT('Ctrl Pts',(-0.294480979947379,-0.0126213686011803,
-4.63290283115898));
#27602=CARTESIAN_POINT('Ctrl Pts',(-0.294662906487123,-0.00636802406559657,
-4.63324260972501));
#27603=CARTESIAN_POINT('Ctrl Pts',(-0.294632262618422,-0.000112863968801113,
-4.63358238829104));
#27604=CARTESIAN_POINT('Ctrl Pts',(-0.294657663022813,-8.13145974722069E-5,
-4.64801761170896));
#27605=CARTESIAN_POINT('Ctrl Pts',(-0.294673906935292,-0.00450595817486475,
-4.64777721106128));
#27606=CARTESIAN_POINT('Ctrl Pts',(-0.294582880583495,-0.00892991872281405,
-4.6475368104136));
#27607=CARTESIAN_POINT('Ctrl Pts',(-0.294382498755337,-0.0133489204924204,
-4.64729640976593));
#27608=CARTESIAN_POINT('Ctrl Pts',(-0.289968779852495,-0.110684251851997,
-4.64200121462443));
#27609=CARTESIAN_POINT('Ctrl Pts',(-0.232499219198468,-0.205613739738578,
-4.63670601948293));
#27610=CARTESIAN_POINT('Ctrl Pts',(-0.148301618536078,-0.254648540524639,
-4.63141082434142));
#27611=CARTESIAN_POINT('Ctrl Pts',(-0.0641040178736896,-0.303683341310699,
-4.62611562919992));
#27612=CARTESIAN_POINT('Ctrl Pts',(0.0468216227970628,-0.306823454996241,
-4.62082043405841));
#27613=CARTESIAN_POINT('Ctrl Pts',(0.133658345028275,-0.262630341080485,
-4.61552523891691));
#27614=CARTESIAN_POINT('Ctrl Pts',(0.220495067259488,-0.218437227164728,
-4.61023004377541));
#27615=CARTESIAN_POINT('Ctrl Pts',(0.283242871051162,-0.126910885647671,
-4.60493484863391));
#27616=CARTESIAN_POINT('Ctrl Pts',(0.293155900001679,-0.029981119824895,
-4.59963965349241));
#27617=CARTESIAN_POINT('Ctrl Pts',(0.303068928952196,0.0669486459978793,
-4.59434445835091));
#27618=CARTESIAN_POINT('Ctrl Pts',(0.260147183061562,0.16928183612637,-4.5890492632094));
#27619=CARTESIAN_POINT('Ctrl Pts',(0.184053858000735,0.230137842622187,
-4.5837540680679));
#27620=CARTESIAN_POINT('Ctrl Pts',(0.107960532939904,0.290993849118007,
-4.5784588729264));
#27621=CARTESIAN_POINT('Ctrl Pts',(-0.00130437129112189,0.310372671981147,
-4.5731636777849));
#27622=CARTESIAN_POINT('Ctrl Pts',(-0.0936847083897634,0.279396536602861,
-4.5678684826434));
#27623=CARTESIAN_POINT('Ctrl Pts',(-0.186065045488401,0.248420401224577,
-4.56257328750189));
#27624=CARTESIAN_POINT('Ctrl Pts',(-0.261560815454657,0.167089307604873,
-4.55727809236039));
#27625=CARTESIAN_POINT('Ctrl Pts',(-0.285586097646837,0.0726624392833101,
-4.55198289721889));
#27626=CARTESIAN_POINT('Ctrl Pts',(-0.291583176180787,0.0490920462069799,
-4.55066113538224));
#27627=CARTESIAN_POINT('Ctrl Pts',(-0.294373241412294,0.024705684106633,
-4.5493393735456));
#27628=CARTESIAN_POINT('Ctrl Pts',(-0.294151842938781,0.000269461638096479,
-4.54801761170896));
#27629=CARTESIAN_POINT('Origin',(0.,0.,-4.78));
#27630=CARTESIAN_POINT('',(-0.293722896168541,-4.16502199041546E-5,-4.43358238829104));
#27631=CARTESIAN_POINT('',(-0.293733435156352,-7.13230564683106E-5,-4.44801761170896));
#27632=CARTESIAN_POINT('',(-0.2942,-3.60291088309151E-17,-4.78));
#27633=CARTESIAN_POINT('Ctrl Pts',(-0.293722896168541,-4.16502199041546E-5,
-4.43358238829104));
#27634=CARTESIAN_POINT('Ctrl Pts',(-0.293657654434464,0.0516276781612295,
-4.43636693469365));
#27635=CARTESIAN_POINT('Ctrl Pts',(-0.280691921537164,0.103327620603503,
-4.43915148109626));
#27636=CARTESIAN_POINT('Ctrl Pts',(-0.25501651195302,0.147667990887853,
-4.44193602749886));
#27637=CARTESIAN_POINT('Ctrl Pts',(-0.206191215323489,0.23198725850077,
-4.44723122264037));
#27638=CARTESIAN_POINT('Ctrl Pts',(-0.111404912997885,0.28969268327525,
-4.45252641778187));
#27639=CARTESIAN_POINT('Ctrl Pts',(-0.0140808528166932,0.294348410027122,
-4.45782161292337));
#27640=CARTESIAN_POINT('Ctrl Pts',(0.0832432073645018,0.299004136778995,
-4.46311680806487));
#27641=CARTESIAN_POINT('Ctrl Pts',(0.183105025401282,0.250610165508259,
-4.46841200320637));
#27642=CARTESIAN_POINT('Ctrl Pts',(0.239756171741916,0.171336613171852,
-4.47370719834788));
#27643=CARTESIAN_POINT('Ctrl Pts',(0.296407318082549,0.0920630608354474,
-4.47900239348938));
#27644=CARTESIAN_POINT('Ctrl Pts',(0.309847792727033,-0.0180900725666295,
-4.48429758863088));
#27645=CARTESIAN_POINT('Ctrl Pts',(0.273920281303337,-0.108659727554603,
-4.48959278377238));
#27646=CARTESIAN_POINT('Ctrl Pts',(0.237992769879641,-0.199229382542577,
-4.49488797891389));
#27647=CARTESIAN_POINT('Ctrl Pts',(0.152697272387766,-0.270215559116452,
-4.50018317405539));
#27648=CARTESIAN_POINT('Ctrl Pts',(0.0571091344883531,-0.289098259523525,
-4.50547836919689));
#27649=CARTESIAN_POINT('Ctrl Pts',(-0.0384790034110612,-0.307980959930598,
-4.5107735643384));
#27650=CARTESIAN_POINT('Ctrl Pts',(-0.144359781718014,-0.274760184170866,
-4.5160687594799));
#27651=CARTESIAN_POINT('Ctrl Pts',(-0.212027380866164,-0.204654945370432,
-4.5213639546214));
#27652=CARTESIAN_POINT('Ctrl Pts',(-0.264074066567786,-0.150733343661248,
-4.52543676584461));
#27653=CARTESIAN_POINT('Ctrl Pts',(-0.293514019904086,-0.0749910716295408,
-4.52950957706782));
#27654=CARTESIAN_POINT('Ctrl Pts',(-0.294207300827486,0.000269263671129533,
-4.53358238829104));
#27655=CARTESIAN_POINT('Ctrl Pts',(-0.294151842938781,0.000269461638096479,
-4.54801761170896));
#27656=CARTESIAN_POINT('Ctrl Pts',(-0.293486282741844,-0.0731898390541624,
-4.5440441784041));
#27657=CARTESIAN_POINT('Ctrl Pts',(-0.26560605257346,-0.147099729093613,
-4.54007074509924));
#27658=CARTESIAN_POINT('Ctrl Pts',(-0.215823605232151,-0.200647503538783,
-4.53609731179438));
#27659=CARTESIAN_POINT('Ctrl Pts',(-0.149481036207181,-0.27200793501589,
-4.53080211665288));
#27660=CARTESIAN_POINT('Ctrl Pts',(-0.0442411037391331,-0.307206154946681,
-4.52550692151137));
#27661=CARTESIAN_POINT('Ctrl Pts',(0.0516839551909757,-0.290117248759129,
-4.52021172636987));
#27662=CARTESIAN_POINT('Ctrl Pts',(0.147609014121084,-0.273028342571577,
-4.51491653122837));
#27663=CARTESIAN_POINT('Ctrl Pts',(0.234219199513256,-0.203652310265684,
-4.50962133608687));
#27664=CARTESIAN_POINT('Ctrl Pts',(0.271836884394817,-0.113771514599516,
-4.50432614094537));
#27665=CARTESIAN_POINT('Ctrl Pts',(0.309454569276379,-0.0238907189333472,
-4.49903094580387));
#27666=CARTESIAN_POINT('Ctrl Pts',(0.298079753647327,0.0864948400930953,
-4.49373575066236));
#27667=CARTESIAN_POINT('Ctrl Pts',(0.242923437684707,0.166815624793344,
-4.48844055552086));
#27668=CARTESIAN_POINT('Ctrl Pts',(0.187767121722086,0.247136409493592,
-4.48314536037936));
#27669=CARTESIAN_POINT('Ctrl Pts',(0.0888293054258945,0.297392419867646,
-4.47785016523786));
#27670=CARTESIAN_POINT('Ctrl Pts',(-0.00856488286340162,0.294560506574261,
-4.47255497009635));
#27671=CARTESIAN_POINT('Ctrl Pts',(-0.105959071152695,0.291728593280876,
-4.46725977495485));
#27672=CARTESIAN_POINT('Ctrl Pts',(-0.201809631435093,0.235808756320058,
-4.46196457981334));
#27673=CARTESIAN_POINT('Ctrl Pts',(-0.252205760855412,0.152418842152444,
-4.45666938467184));
#27674=CARTESIAN_POINT('Ctrl Pts',(-0.279653025674511,0.107002158694258,
-4.45378546035088));
#27675=CARTESIAN_POINT('Ctrl Pts',(-0.293617493229099,0.0534372380940554,
-4.45090153602992));
#27676=CARTESIAN_POINT('Ctrl Pts',(-0.293733435156352,-7.13230564683106E-5,
-4.44801761170896));
#27677=CARTESIAN_POINT('Origin',(0.,0.,-4.78));
#27678=CARTESIAN_POINT('',(-0.294360370562084,-0.000249476265296811,-4.33358238829104));
#27679=CARTESIAN_POINT('',(-0.294413795075237,-0.00023539599080995,-4.34801761170896));
#27680=CARTESIAN_POINT('',(-0.2942,-3.60291088309151E-17,-4.78));
#27681=CARTESIAN_POINT('Ctrl Pts',(-0.294360370562084,-0.000249476265296811,
-4.33358238829104));
#27682=CARTESIAN_POINT('Ctrl Pts',(-0.293636096245715,0.0799648134312458,
-4.33792909717797));
#27683=CARTESIAN_POINT('Ctrl Pts',(-0.259626145442727,0.160719405307108,
-4.3422758060649));
#27684=CARTESIAN_POINT('Ctrl Pts',(-0.201183530857245,0.215324043741873,
-4.34662251495182));
#27685=CARTESIAN_POINT('Ctrl Pts',(-0.129988275582514,0.281843846117607,
-4.35191771009333));
#27686=CARTESIAN_POINT('Ctrl Pts',(-0.02253420186159,0.30955631980262,-4.35721290523483));
#27687=CARTESIAN_POINT('Ctrl Pts',(0.0719521168432027,0.285765900315839,
-4.36250810037633));
#27688=CARTESIAN_POINT('Ctrl Pts',(0.166438435547995,0.261975480829059,
-4.36780329551783));
#27689=CARTESIAN_POINT('Ctrl Pts',(0.247956999236658,0.186682168170484,
-4.37309849065933));
#27690=CARTESIAN_POINT('Ctrl Pts',(0.279162741081986,0.0943791337803656,
-4.37839368580084));
#27691=CARTESIAN_POINT('Ctrl Pts',(0.310368482927314,0.00207609939024855,
-4.38368888094234));
#27692=CARTESIAN_POINT('Ctrl Pts',(0.29126140292931,-0.107236656731413,
-4.38898407608384));
#27693=CARTESIAN_POINT('Ctrl Pts',(0.230594785580612,-0.183481066501619,
-4.39427927122535));
#27694=CARTESIAN_POINT('Ctrl Pts',(0.169928168231914,-0.259725476271827,
-4.39957446636685));
#27695=CARTESIAN_POINT('Ctrl Pts',(0.067702013532521,-0.302901539690579,
-4.40486966150834));
#27696=CARTESIAN_POINT('Ctrl Pts',(-0.0292521053642755,-0.293229553819695,
-4.41016485664985));
#27697=CARTESIAN_POINT('Ctrl Pts',(-0.126206224261071,-0.283557567948812,
-4.41546005179135));
#27698=CARTESIAN_POINT('Ctrl Pts',(-0.217888307355266,-0.221037532788297,
-4.42075524693286));
#27699=CARTESIAN_POINT('Ctrl Pts',(-0.262297203435638,-0.134310959982362,
-4.42605044207436));
#27700=CARTESIAN_POINT('Ctrl Pts',(-0.283353110906546,-0.093190669827754,
-4.42856109081325));
#27701=CARTESIAN_POINT('Ctrl Pts',(-0.293781720498863,-0.0466286038501627,
-4.43107173955215));
#27702=CARTESIAN_POINT('Ctrl Pts',(-0.293722896168541,-4.16502199041546E-5,
-4.43358238829104));
#27703=CARTESIAN_POINT('Ctrl Pts',(-0.293733435156352,-7.13230564683106E-5,
-4.44801761170896));
#27704=CARTESIAN_POINT('Ctrl Pts',(-0.29383037507396,-0.0448102335797182,
-4.44560634088842));
#27705=CARTESIAN_POINT('Ctrl Pts',(-0.284246145997896,-0.0895097445761582,
-4.44319507006788));
#27706=CARTESIAN_POINT('Ctrl Pts',(-0.264766978775821,-0.129374248603317,
-4.44078379924734));
#27707=CARTESIAN_POINT('Ctrl Pts',(-0.221990368717675,-0.216917433817043,
-4.43548860410584));
#27708=CARTESIAN_POINT('Ctrl Pts',(-0.131495450043148,-0.281143812870087,
-4.43019340896433));
#27709=CARTESIAN_POINT('Ctrl Pts',(-0.0347395133680276,-0.292630168408354,
-4.42489821382283));
#27710=CARTESIAN_POINT('Ctrl Pts',(0.0620164233070968,-0.304116523946622,
-4.41960301868133));
#27711=CARTESIAN_POINT('Ctrl Pts',(0.165033377982814,-0.262862855970111,
-4.41430782353983));
#27712=CARTESIAN_POINT('Ctrl Pts',(0.227117498331296,-0.187768184747797,
-4.40901262839833));
#27713=CARTESIAN_POINT('Ctrl Pts',(0.289201618679778,-0.112673513525485,
-4.40371743325683));
#27714=CARTESIAN_POINT('Ctrl Pts',(0.310352904701023,-0.00373783905737107,
-4.39842223811532));
#27715=CARTESIAN_POINT('Ctrl Pts',(0.280881585694931,0.0891335182142501,
-4.39312704297382));
#27716=CARTESIAN_POINT('Ctrl Pts',(0.25141026668884,0.18200487548587,-4.38783184783232));
#27717=CARTESIAN_POINT('Ctrl Pts',(0.171316342655413,0.258811915561,-4.38253665269081));
#27718=CARTESIAN_POINT('Ctrl Pts',(0.0772922283053036,0.284368002235396,
-4.37724145754931));
#27719=CARTESIAN_POINT('Ctrl Pts',(-0.0167318860448084,0.309924088909792,
-4.37194626240781));
#27720=CARTESIAN_POINT('Ctrl Pts',(-0.124686190711601,0.284229222183455,
-4.36665106726631));
#27721=CARTESIAN_POINT('Ctrl Pts',(-0.197114947766929,0.219054665822461,
-4.36135587212481));
#27722=CARTESIAN_POINT('Ctrl Pts',(-0.257929428151737,0.164331142452089,
-4.35690978531953));
#27723=CARTESIAN_POINT('Ctrl Pts',(-0.293698234899642,0.081774257223651,
-4.35246369851424));
#27724=CARTESIAN_POINT('Ctrl Pts',(-0.294413795075237,-0.00023539599080995,
-4.34801761170896));
#27725=CARTESIAN_POINT('Origin',(0.,0.,-4.78));
#27726=CARTESIAN_POINT('',(-0.294529459134955,0.000188340711244316,-4.23358238829104));
#27727=CARTESIAN_POINT('',(-0.294482957137414,0.000210451042227086,-4.24801761170896));
#27728=CARTESIAN_POINT('',(-0.2942,-3.60291088309151E-17,-4.78));
#27729=CARTESIAN_POINT('Ctrl Pts',(-0.294529459134955,0.000188340711244316,
-4.23358238829104));
#27730=CARTESIAN_POINT('Ctrl Pts',(-0.294613692761748,0.0114962305757796,
-4.23419606452079));
#27731=CARTESIAN_POINT('Ctrl Pts',(-0.294018958340253,0.0227951767893906,
-4.23480974075053));
#27732=CARTESIAN_POINT('Ctrl Pts',(-0.292715655427141,0.0340117916229041,
-4.23542341698028));
#27733=CARTESIAN_POINT('Ctrl Pts',(-0.281469915541974,0.130795993929768,
-4.24071861212178));
#27734=CARTESIAN_POINT('Ctrl Pts',(-0.217468745024552,0.221450333756189,
-4.24601380726328));
#27735=CARTESIAN_POINT('Ctrl Pts',(-0.130032189295706,0.264444486893763,
-4.25130900240478));
#27736=CARTESIAN_POINT('Ctrl Pts',(-0.0425956335668611,0.307438640031337,
-4.25660419754628));
#27737=CARTESIAN_POINT('Ctrl Pts',(0.0682763073734012,0.302772606480067,
-4.26189939268779));
#27738=CARTESIAN_POINT('Ctrl Pts',(0.151791275854399,0.252583977076999,
-4.26719458782929));
#27739=CARTESIAN_POINT('Ctrl Pts',(0.235306244335397,0.202395347673931,
-4.27248978297079));
#27740=CARTESIAN_POINT('Ctrl Pts',(0.291464240357126,0.106684122419057,
-4.27778497811229));
#27741=CARTESIAN_POINT('Ctrl Pts',(0.294538312665593,0.00929727237664749,
-4.28308017325379));
#27742=CARTESIAN_POINT('Ctrl Pts',(0.297612384974061,-0.0880895776657633,
-4.2883753683953));
#27743=CARTESIAN_POINT('Ctrl Pts',(0.24760253356927,-0.187152052495716,
-4.2936705635368));
#27744=CARTESIAN_POINT('Ctrl Pts',(0.167419138102454,-0.242507915537971,
-4.2989657586783));
#27745=CARTESIAN_POINT('Ctrl Pts',(0.0872357426356381,-0.297863778580225,
-4.30426095381981));
#27746=CARTESIAN_POINT('Ctrl Pts',(-0.0231211968932015,-0.309513029834782,
-4.30955614896131));
#27747=CARTESIAN_POINT('Ctrl Pts',(-0.113095253885456,-0.272118945408298,
-4.31485134410281));
#27748=CARTESIAN_POINT('Ctrl Pts',(-0.203069310877712,-0.234724860981814,
-4.32014653924431));
#27749=CARTESIAN_POINT('Ctrl Pts',(-0.272660485333381,-0.148287440874289,
-4.32544173438581));
#27750=CARTESIAN_POINT('Ctrl Pts',(-0.289987854146947,-0.0524051652872991,
-4.33073692952732));
#27751=CARTESIAN_POINT('Ctrl Pts',(-0.293091568119413,-0.0352305346983667,
-4.33168541578189));
#27752=CARTESIAN_POINT('Ctrl Pts',(-0.294518412945755,-0.0177528686425654,
-4.33263390203647));
#27753=CARTESIAN_POINT('Ctrl Pts',(-0.294360370562084,-0.000249476265296811,
-4.33358238829104));
#27754=CARTESIAN_POINT('Ctrl Pts',(-0.294413795075237,-0.00023539599080995,
-4.34801761170896));
#27755=CARTESIAN_POINT('Ctrl Pts',(-0.294550451901065,-0.0158975013982573,
-4.34716850337274));
#27756=CARTESIAN_POINT('Ctrl Pts',(-0.293408615057636,-0.0315396476654283,
-4.34631939503652));
#27757=CARTESIAN_POINT('Ctrl Pts',(-0.29091857628131,-0.0469641483070301,
-4.3454702867003));
#27758=CARTESIAN_POINT('Ctrl Pts',(-0.275390238296502,-0.143154160079883,
-4.34017509155879));
#27759=CARTESIAN_POINT('Ctrl Pts',(-0.207430352883024,-0.230879937629941,
-4.33487989641729));
#27760=CARTESIAN_POINT('Ctrl Pts',(-0.118172521364231,-0.269952781882628,
-4.32958470127579));
#27761=CARTESIAN_POINT('Ctrl Pts',(-0.0289146898454392,-0.309025626135314,
-4.32428950613429));
#27762=CARTESIAN_POINT('Ctrl Pts',(0.0816410877786669,-0.299445537090632,
-4.31899431099279));
#27763=CARTESIAN_POINT('Ctrl Pts',(0.162847293731964,-0.245601319572848,
-4.31369911585128));
#27764=CARTESIAN_POINT('Ctrl Pts',(0.244053499685263,-0.191757102055065,
-4.30840392070978));
#27765=CARTESIAN_POINT('Ctrl Pts',(0.295910133967752,-0.0936487560641784,
-4.30310872556828));
#27766=CARTESIAN_POINT('Ctrl Pts',(0.29466077368526,0.00377858478179017,
-4.29781353042678));
#27767=CARTESIAN_POINT('Ctrl Pts',(0.293411413402767,0.101205925627759,
-4.29251833528528));
#27768=CARTESIAN_POINT('Ctrl Pts',(0.239056058555293,0.19795226132881,-4.28722314014377));
#27769=CARTESIAN_POINT('Ctrl Pts',(0.156495839233253,0.24969641878575,-4.28192794500227));
#27770=CARTESIAN_POINT('Ctrl Pts',(0.0739356199112137,0.301440576242691,
-4.27663274986077));
#27771=CARTESIAN_POINT('Ctrl Pts',(-0.0368294638853918,0.308182555455522,
-4.27133755471927));
#27772=CARTESIAN_POINT('Ctrl Pts',(-0.125056007595323,0.266833738901338,
-4.26604235957776));
#27773=CARTESIAN_POINT('Ctrl Pts',(-0.213282551305254,0.225484922347155,
-4.26074716443626));
#27774=CARTESIAN_POINT('Ctrl Pts',(-0.278970554928511,0.13604531002596,
-4.25545196929476));
#27775=CARTESIAN_POINT('Ctrl Pts',(-0.292027205563913,0.0394887384235212,
-4.25015677415325));
#27776=CARTESIAN_POINT('Ctrl Pts',(-0.293785421955766,0.0264863726810973,
-4.24944372000516));
#27777=CARTESIAN_POINT('Ctrl Pts',(-0.294589248926741,0.0133549517223198,
-4.24873066585706));
#27778=CARTESIAN_POINT('Ctrl Pts',(-0.294482957137414,0.000210451042227086,
-4.24801761170896));
#27779=CARTESIAN_POINT('Origin',(0.,0.,-4.78));
#27780=CARTESIAN_POINT('',(-0.293780102848547,0.000137479377752783,-4.13358238829104));
#27781=CARTESIAN_POINT('',(-0.293756768933342,0.000110456432129071,-4.14801761170896));
#27782=CARTESIAN_POINT('',(-0.2942,-3.60291088309151E-17,-4.78));
#27783=CARTESIAN_POINT('Ctrl Pts',(-0.293780102848547,0.000137479377752783,
-4.13358238829104));
#27784=CARTESIAN_POINT('Ctrl Pts',(-0.293950256150424,0.0404921514148337,
-4.13575822700511));
#27785=CARTESIAN_POINT('Ctrl Pts',(-0.286209896249464,0.0807843543255878,
-4.13793406571917));
#27786=CARTESIAN_POINT('Ctrl Pts',(-0.270245791604979,0.1175009320021,-4.14010990443324));
#27787=CARTESIAN_POINT('Ctrl Pts',(-0.231395003260468,0.206855644954183,
-4.14540509957474));
#27788=CARTESIAN_POINT('Ctrl Pts',(-0.143838473188879,0.275033450718222,
-4.15070029471624));
#27789=CARTESIAN_POINT('Ctrl Pts',(-0.0476873652618052,0.29080091488151,
-4.15599548985774));
#27790=CARTESIAN_POINT('Ctrl Pts',(0.0484637426652683,0.306568379044798,
-4.16129068499924));
#27791=CARTESIAN_POINT('Ctrl Pts',(0.153209428447825,0.269925501607335,
-4.16658588014074));
#27792=CARTESIAN_POINT('Ctrl Pts',(0.218563878077358,0.197659019782356,
-4.17188107528225));
#27793=CARTESIAN_POINT('Ctrl Pts',(0.283918327706889,0.12539253795738,-4.17717627042375));
#27794=CARTESIAN_POINT('Ctrl Pts',(0.309881541183399,0.017502451744889,
-4.18247146556526));
#27795=CARTESIAN_POINT('Ctrl Pts',(0.284559320443789,-0.0765849205138502,
-4.18776666070676));
#27796=CARTESIAN_POINT('Ctrl Pts',(0.259237099704177,-0.170672292772595,
-4.19306185584826));
#27797=CARTESIAN_POINT('Ctrl Pts',(0.18262944474844,-0.250956951077586,
-4.19835705098976));
#27798=CARTESIAN_POINT('Ctrl Pts',(0.0898316500020959,-0.280659102042746,
-4.20365224613126));
#27799=CARTESIAN_POINT('Ctrl Pts',(-0.0029661447442441,-0.310361253007904,
-4.20894744127276));
#27800=CARTESIAN_POINT('Ctrl Pts',(-0.111954079281189,-0.289480896633235,
-4.21424263641427));
#27801=CARTESIAN_POINT('Ctrl Pts',(-0.187202891923205,-0.227583686052249,
-4.21953783155577));
#27802=CARTESIAN_POINT('Ctrl Pts',(-0.253730891374979,-0.172859930991974,
-4.22421935046753));
#27803=CARTESIAN_POINT('Ctrl Pts',(-0.293886870587892,-0.0860755516916222,
-4.22890086937928));
#27804=CARTESIAN_POINT('Ctrl Pts',(-0.294529459134955,0.000188340711244316,
-4.23358238829104));
#27805=CARTESIAN_POINT('Ctrl Pts',(-0.294482957137414,0.000210451042227086,
-4.24801761170896));
#27806=CARTESIAN_POINT('Ctrl Pts',(-0.293799917894968,-0.0842571248980618,
-4.24343547071556));
#27807=CARTESIAN_POINT('Ctrl Pts',(-0.255534008629857,-0.169264820971633,
-4.23885332972216));
#27808=CARTESIAN_POINT('Ctrl Pts',(-0.191432955524924,-0.224037212959682,
-4.23427118872875));
#27809=CARTESIAN_POINT('Ctrl Pts',(-0.117356757202993,-0.287333061856756,
-4.22897599358725));
#27810=CARTESIAN_POINT('Ctrl Pts',(-0.00877906291158649,-0.310251228767228,
-4.22368079844574));
#27811=CARTESIAN_POINT('Ctrl Pts',(0.0845588038301234,-0.282292504233761,
-4.21838560330424));
#27812=CARTESIAN_POINT('Ctrl Pts',(0.177896670571836,-0.254333779700292,
-4.21309040816274));
#27813=CARTESIAN_POINT('Ctrl Pts',(0.255994709763852,-0.175498163722882,
-4.20779521302124));
#27814=CARTESIAN_POINT('Ctrl Pts',(0.283074856132123,-0.081901618283934,
-4.20250001787973));
#27815=CARTESIAN_POINT('Ctrl Pts',(0.310155002500395,0.0116949271550137,
-4.19720482273823));
#27816=CARTESIAN_POINT('Ctrl Pts',(0.286217256044923,0.120052402055498,
-4.19190962759673));
#27817=CARTESIAN_POINT('Ctrl Pts',(0.222227913282986,0.193530369217956,
-4.18661443245523));
#27818=CARTESIAN_POINT('Ctrl Pts',(0.158238570521051,0.267008336380412,
-4.18131923731373));
#27819=CARTESIAN_POINT('Ctrl Pts',(0.0541976314526524,0.305606795804842,
-4.17602404217222));
#27820=CARTESIAN_POINT('Ctrl Pts',(-0.0422319465973879,0.291643124277504,
-4.17072884703072));
#27821=CARTESIAN_POINT('Ctrl Pts',(-0.138661524647431,0.277679452750165,
-4.16543365188922));
#27822=CARTESIAN_POINT('Ctrl Pts',(-0.227479741679115,0.211153650271055,
-4.16013845674772));
#27823=CARTESIAN_POINT('Ctrl Pts',(-0.267997433158201,0.12254233991714,
-4.15484326160622));
#27824=CARTESIAN_POINT('Ctrl Pts',(-0.285406900249956,0.0844682138934502,
-4.1525680449738));
#27825=CARTESIAN_POINT('Ctrl Pts',(-0.293899066372842,0.0423166349121218,
-4.15029282834138));
#27826=CARTESIAN_POINT('Ctrl Pts',(-0.293756768933342,0.000110456432129071,
-4.14801761170896));
#27827=CARTESIAN_POINT('Origin',(0.,0.,-4.78));
#27828=CARTESIAN_POINT('',(-0.294026166038071,-0.000255545996156264,-4.03358238829104));
#27829=CARTESIAN_POINT('',(-0.294077901483341,-0.000263827746408872,-4.04801761170896));
#27830=CARTESIAN_POINT('',(-0.2942,-3.60291088309151E-17,-4.78));
#27831=CARTESIAN_POINT('Ctrl Pts',(-0.294026166038071,-0.000255545996156264,
-4.03358238829104));
#27832=CARTESIAN_POINT('Ctrl Pts',(-0.293452221785546,0.0689262477218108,
-4.03732038948942));
#27833=CARTESIAN_POINT('Ctrl Pts',(-0.26906437292607,0.138472261120715,
-4.04105839068781));
#27834=CARTESIAN_POINT('Ctrl Pts',(-0.224512522408552,0.190875310567925,
-4.04479639188619));
#27835=CARTESIAN_POINT('Ctrl Pts',(-0.16140105457187,0.265108666339113,
-4.05009158702769));
#27836=CARTESIAN_POINT('Ctrl Pts',(-0.0578262408769573,0.304941029133992,
-4.05538678216919));
#27837=CARTESIAN_POINT('Ctrl Pts',(0.038762501456049,0.292124503221433,
-4.0606819773107));
#27838=CARTESIAN_POINT('Ctrl Pts',(0.135351243789059,0.279307977308873,
-4.0659771724522));
#27839=CARTESIAN_POINT('Ctrl Pts',(0.22495391476016,0.213842562688867,-4.07127236759371));
#27840=CARTESIAN_POINT('Ctrl Pts',(0.266521977893879,0.125719100381765,
-4.07656756273521));
#27841=CARTESIAN_POINT('Ctrl Pts',(0.308090041027596,0.0375956380746656,
-4.08186275787671));
#27842=CARTESIAN_POINT('Ctrl Pts',(0.301623496323935,-0.0731858719195301,
-4.08715795301821));
#27843=CARTESIAN_POINT('Ctrl Pts',(0.250084779981618,-0.155874499913395,
-4.09245314815971));
#27844=CARTESIAN_POINT('Ctrl Pts',(0.198546063639301,-0.238563127907258,
-4.09774834330121));
#27845=CARTESIAN_POINT('Ctrl Pts',(0.10193517565833,-0.293158873900794,
-4.10304353844272));
#27846=CARTESIAN_POINT('Ctrl Pts',(0.00451123819089411,-0.294650480453547,
-4.10833873358422));
#27847=CARTESIAN_POINT('Ctrl Pts',(-0.092912699276546,-0.296142087006301,
-4.11363392872572));
#27848=CARTESIAN_POINT('Ctrl Pts',(-0.191149686230449,-0.24452955411827,
-4.11892912386722));
#27849=CARTESIAN_POINT('Ctrl Pts',(-0.245195656398686,-0.16345747760419,
-4.12422431900872));
#27850=CARTESIAN_POINT('Ctrl Pts',(-0.277033698230241,-0.115698576146939,
-4.12734367543616));
#27851=CARTESIAN_POINT('Ctrl Pts',(-0.293536165284412,-0.0577163517827691,
-4.1304630318636));
#27852=CARTESIAN_POINT('Ctrl Pts',(-0.293780102848547,0.000137479377752783,
-4.13358238829104));
#27853=CARTESIAN_POINT('Ctrl Pts',(-0.293756768933342,0.000110456432129071,
-4.14801761170896));
#27854=CARTESIAN_POINT('Ctrl Pts',(-0.293567892321301,-0.0559113527195887,
-4.14499763319988));
#27855=CARTESIAN_POINT('Ctrl Pts',(-0.278166621949572,-0.112029356506533,
-4.14197765469079));
#27856=CARTESIAN_POINT('Ctrl Pts',(-0.248214382111388,-0.158835983847513,
-4.13895767618171));
#27857=CARTESIAN_POINT('Ctrl Pts',(-0.195696473658997,-0.240906179029544,
-4.13366248104021));
#27858=CARTESIAN_POINT('Ctrl Pts',(-0.0984434908277233,-0.294349751164889,
-4.1283672858987));
#27859=CARTESIAN_POINT('Ctrl Pts',(-0.00100871054776456,-0.294683273625728,
-4.1230720907572));
#27860=CARTESIAN_POINT('Ctrl Pts',(0.0964260697321914,-0.295016796086566,
-4.1177768956157));
#27861=CARTESIAN_POINT('Ctrl Pts',(0.194042647460834,-0.242240268872898,
-4.1124817004742));
#27862=CARTESIAN_POINT('Ctrl Pts',(0.247121176583794,-0.16053153377332,
-4.1071865053327));
#27863=CARTESIAN_POINT('Ctrl Pts',(0.300199705706755,-0.0788227986737399,
-4.1018913101912));
#27864=CARTESIAN_POINT('Ctrl Pts',(0.308740186224036,0.0318181443117522,
-4.09659611504969));
#27865=CARTESIAN_POINT('Ctrl Pts',(0.268830075995526,0.12070476167888,-4.09130091990819));
#27866=CARTESIAN_POINT('Ctrl Pts',(0.228919965767017,0.209591379046007,
-4.08600572476668));
#27867=CARTESIAN_POINT('Ctrl Pts',(0.140559264792717,0.27672367079477,-4.08071052962518));
#27868=CARTESIAN_POINT('Ctrl Pts',(0.0442275415712278,0.291347170602866,
-4.07541533448368));
#27869=CARTESIAN_POINT('Ctrl Pts',(-0.0521041816502612,0.305970670410962,
-4.07012013934218));
#27870=CARTESIAN_POINT('Ctrl Pts',(-0.156406927118939,0.268085378278393,
-4.06482494420068));
#27871=CARTESIAN_POINT('Ctrl Pts',(-0.220897799459659,0.195047203122207,
-4.05952974905918));
#27872=CARTESIAN_POINT('Ctrl Pts',(-0.267633740275297,0.142117110731031,
-4.05569236994244));
#27873=CARTESIAN_POINT('Ctrl Pts',(-0.293461411669798,0.0707255421157874,
-4.0518549908257));
#27874=CARTESIAN_POINT('Ctrl Pts',(-0.294077901483341,-0.000263827746408872,
-4.04801761170896));
#27875=CARTESIAN_POINT('Origin',(0.,0.,-4.78));
#27876=CARTESIAN_POINT('',(-0.294685005132684,1.71253444288745E-6,-3.93358238829104));
#27877=CARTESIAN_POINT('',(-0.294679608262217,3.58352270703291E-5,-3.94801761170896));
#27878=CARTESIAN_POINT('',(-0.2942,-3.60291088309151E-17,-4.78));
#27879=CARTESIAN_POINT('Ctrl Pts',(-0.294685000185643,1.71251697507702E-6,
-3.93358238829104));
#27880=CARTESIAN_POINT('Ctrl Pts',(-0.2946934016704,0.097528503871605,-3.93888255197374));
#27881=CARTESIAN_POINT('Ctrl Pts',(-0.241468922813224,0.195047402076887,
-3.94418271565645));
#27882=CARTESIAN_POINT('Ctrl Pts',(-0.159452677353124,0.247818684994796,
-3.94948287933915));
#27883=CARTESIAN_POINT('Ctrl Pts',(-0.0775133165175665,0.300540498441735,
-3.95477807448065));
#27884=CARTESIAN_POINT('Ctrl Pts',(0.0331638128330922,0.308598552980046,
-3.96007326962216));
#27885=CARTESIAN_POINT('Ctrl Pts',(0.121875599210725,0.268301314246642,
-3.96536846476366));
#27886=CARTESIAN_POINT('Ctrl Pts',(0.210587385588363,0.228004075513236,
-3.97066365990516));
#27887=CARTESIAN_POINT('Ctrl Pts',(0.277333828992975,0.139351543508113,
-3.97595885504666));
#27888=CARTESIAN_POINT('Ctrl Pts',(0.291537227113789,0.0429569795443333,
-3.98125405018816));
#27889=CARTESIAN_POINT('Ctrl Pts',(0.305740625234603,-0.0534375844194461,
-3.98654924532967));
#27890=CARTESIAN_POINT('Ctrl Pts',(0.267400978071619,-0.15757418034188,
-3.99184444047117));
#27891=CARTESIAN_POINT('Ctrl Pts',(0.194082342353633,-0.221746028815296,
-3.99713963561267));
#27892=CARTESIAN_POINT('Ctrl Pts',(0.120763706635648,-0.285917877288712,
-4.00243483075417));
#27893=CARTESIAN_POINT('Ctrl Pts',(0.0124660823626598,-0.31012497831311,
-4.00773002589568));
#27894=CARTESIAN_POINT('Ctrl Pts',(-0.0811975118224673,-0.283277639385434,
-4.01302522103718));
#27895=CARTESIAN_POINT('Ctrl Pts',(-0.174861106007593,-0.256430300457758,
-4.01832041617868));
#27896=CARTESIAN_POINT('Ctrl Pts',(-0.25389067010486,-0.17852852157801,
-4.02361561132018));
#27897=CARTESIAN_POINT('Ctrl Pts',(-0.282081391164271,-0.0852604577643881,
-4.02891080646168));
#27898=CARTESIAN_POINT('Ctrl Pts',(-0.290371627673553,-0.0578324857679226,
-4.0304680004048));
#27899=CARTESIAN_POINT('Ctrl Pts',(-0.294265262407036,-0.0290756197292115,
-4.03202519434792));
#27900=CARTESIAN_POINT('Ctrl Pts',(-0.294026166038071,-0.000255545996156264,
-4.03358238829104));
#27901=CARTESIAN_POINT('Ctrl Pts',(-0.294077901483341,-0.000263827746408872,
-4.04801761170896));
#27902=CARTESIAN_POINT('Ctrl Pts',(-0.294312105272423,-0.0272326097782939,
-4.04655979568419));
#27903=CARTESIAN_POINT('Ctrl Pts',(-0.290907751712052,-0.0541433452158874,
-4.04510197965943));
#27904=CARTESIAN_POINT('Ctrl Pts',(-0.283628919847751,-0.0799617726008578,
-4.04364416363466));
#27905=CARTESIAN_POINT('Ctrl Pts',(-0.257190168682364,-0.173741514987928,
-4.03834896849316));
#27906=CARTESIAN_POINT('Ctrl Pts',(-0.179633667138827,-0.253109941582263,
-4.03305377335166));
#27907=CARTESIAN_POINT('Ctrl Pts',(-0.0864893927053731,-0.281707000625053,
-4.02775857821016));
#27908=CARTESIAN_POINT('Ctrl Pts',(0.00665488172808236,-0.310304059667843,
-4.02246338306866));
#27909=CARTESIAN_POINT('Ctrl Pts',(0.115386929051455,-0.288129751159088,
-4.01716818792715));
#27910=CARTESIAN_POINT('Ctrl Pts',(0.189894713939502,-0.225342510127807,
-4.01187299278565));
#27911=CARTESIAN_POINT('Ctrl Pts',(0.264402498827548,-0.162555269096528,
-4.00657779764415));
#27912=CARTESIAN_POINT('Ctrl Pts',(0.304686021280268,-0.0591550955427229,
-4.00128260250265));
#27913=CARTESIAN_POINT('Ctrl Pts',(0.292290701520345,0.0374885989910175,
-3.99598740736115));
#27914=CARTESIAN_POINT('Ctrl Pts',(0.279895381760423,0.134132293524755,
-3.99069221221964));
#27915=CARTESIAN_POINT('Ctrl Pts',(0.214821219787862,0.224019509038431,
-3.98539701707814));
#27916=CARTESIAN_POINT('Ctrl Pts',(0.126879816978892,0.265971354276274,
-3.98010182193664));
#27917=CARTESIAN_POINT('Ctrl Pts',(0.0389384141699212,0.307923199514117,
-3.97480662679514));
#27918=CARTESIAN_POINT('Ctrl Pts',(-0.0718702294754556,0.301939674476127,
-3.96951143165363));
#27919=CARTESIAN_POINT('Ctrl Pts',(-0.154782753823608,0.250761935663777,
-3.96421623651213));
#27920=CARTESIAN_POINT('Ctrl Pts',(-0.237695278171766,0.199584196851422,
-3.95892104137063));
#27921=CARTESIAN_POINT('Ctrl Pts',(-0.292711683222693,0.103212244264697,
-3.95362584622913));
#27922=CARTESIAN_POINT('Ctrl Pts',(-0.294628000429138,0.00579573964666751,
-3.94833065108763));
#27923=CARTESIAN_POINT('Ctrl Pts',(-0.294665763138638,0.00387606207341759,
-3.94822630462807));
#27924=CARTESIAN_POINT('Ctrl Pts',(-0.294682905939502,0.00195597887809947,
-3.94812195816852));
#27925=CARTESIAN_POINT('Ctrl Pts',(-0.294679608262217,3.58352270703291E-5,
-3.94801761170896));
#27926=CARTESIAN_POINT('Origin',(0.,0.,-4.78));
#27927=CARTESIAN_POINT('',(-0.29402112681354,0.000254531718302781,-3.83358238829104));
#27928=CARTESIAN_POINT('',(-0.29397219999165,0.000242578469533487,-3.84801761170896));
#27929=CARTESIAN_POINT('',(-0.2942,-3.60291088309151E-17,-4.78));
#27930=CARTESIAN_POINT('Ctrl Pts',(-0.29402112681354,0.000254531718302781,
-3.83358238829104));
#27931=CARTESIAN_POINT('Ctrl Pts',(-0.294260484629604,0.0292597759619457,
-3.83514951931656));
#27932=CARTESIAN_POINT('Ctrl Pts',(-0.290316015523389,0.0582013467529887,
-3.83671665034208));
#27933=CARTESIAN_POINT('Ctrl Pts',(-0.281921184254449,0.0857886711899819,
-3.8382837813676));
#27934=CARTESIAN_POINT('Ctrl Pts',(-0.253555802531341,0.179003765490896,
-3.84357897650911));
#27935=CARTESIAN_POINT('Ctrl Pts',(-0.17438048147878,0.256757382147876,
-3.84887417165061));
#27936=CARTESIAN_POINT('Ctrl Pts',(-0.0806667692689985,0.283429234222764,
-3.85416936679211));
#27937=CARTESIAN_POINT('Ctrl Pts',(0.013046942940783,0.310101086297652,
-3.85946456193361));
#27938=CARTESIAN_POINT('Ctrl Pts',(0.121299046307785,0.285691173790448,
-3.86475975707511));
#27939=CARTESIAN_POINT('Ctrl Pts',(0.194497356191566,0.221382104600103,
-3.87005495221662));
#27940=CARTESIAN_POINT('Ctrl Pts',(0.267695666075345,0.15707303540976,-3.87535014735812));
#27941=CARTESIAN_POINT('Ctrl Pts',(0.305840182475905,0.052864809536277,
-3.88064534249962));
#27942=CARTESIAN_POINT('Ctrl Pts',(0.291456251676112,-0.0435029807442393,
-3.88594053764112));
#27943=CARTESIAN_POINT('Ctrl Pts',(0.277072320876318,-0.139870771024758,
-3.89123573278263));
#27944=CARTESIAN_POINT('Ctrl Pts',(0.210159942876168,-0.22839812571231,
-3.89653092792413));
#27945=CARTESIAN_POINT('Ctrl Pts',(0.121372832354126,-0.268529128301459,
-3.90182612306563));
#27946=CARTESIAN_POINT('Ctrl Pts',(0.0325857218320838,-0.308660130890608,
-3.90712131820713));
#27947=CARTESIAN_POINT('Ctrl Pts',(-0.0780761212118509,-0.300394781381353,
-3.91241651334864));
#27948=CARTESIAN_POINT('Ctrl Pts',(-0.159916585829454,-0.247519580175258,
-3.91771170849014));
#27949=CARTESIAN_POINT('Ctrl Pts',(-0.241680258617952,-0.194693992365591,
-3.92300193509044));
#27950=CARTESIAN_POINT('Ctrl Pts',(-0.294676614452523,-0.0973422294352269,
-3.92829216169074));
#27951=CARTESIAN_POINT('Ctrl Pts',(-0.294685000185643,1.71251697507702E-6,
-3.93358238829104));
#27952=CARTESIAN_POINT('Ctrl Pts',(-0.294679608262217,3.58352270703291E-5,
-3.94801761170896));
#27953=CARTESIAN_POINT('Ctrl Pts',(-0.294515561069259,-0.0954841774555884,
-3.94282676302701));
#27954=CARTESIAN_POINT('Ctrl Pts',(-0.24376760897675,-0.191153799453464,
-3.93763591434507));
#27955=CARTESIAN_POINT('Ctrl Pts',(-0.164524860722765,-0.244480713889306,
-3.93244506566312));
#27956=CARTESIAN_POINT('Ctrl Pts',(-0.0836891744479772,-0.298879606157931,
-3.92714987052162));
#27957=CARTESIAN_POINT('Ctrl Pts',(0.0267984274635758,-0.309216334045853,
-3.92185467538011));
#27958=CARTESIAN_POINT('Ctrl Pts',(0.116321659345001,-0.27075546322323,
-3.91655948023861));
#27959=CARTESIAN_POINT('Ctrl Pts',(0.205844891226431,-0.232294592400605,
-3.91126428509711));
#27960=CARTESIAN_POINT('Ctrl Pts',(0.274403753077735,-0.145036122867431,
-3.90596908995561));
#27961=CARTESIAN_POINT('Ctrl Pts',(0.290590242796307,-0.0489546720638047,
-3.9006738948141));
#27962=CARTESIAN_POINT('Ctrl Pts',(0.30677673251488,0.0471267787398241,
-3.8953786996726));
#27963=CARTESIAN_POINT('Ctrl Pts',(0.270590850100718,0.152031210813905,
-3.8900835045311));
#27964=CARTESIAN_POINT('Ctrl Pts',(0.198609974058795,0.217700086238457,
-3.8847883093896));
#27965=CARTESIAN_POINT('Ctrl Pts',(0.126629098016877,0.283368961663006,
-3.8794931142481));
#27966=CARTESIAN_POINT('Ctrl Pts',(0.0188532283472031,0.309802280438032,
-3.87419791910659));
#27967=CARTESIAN_POINT('Ctrl Pts',(-0.0753436385431076,0.284890480118608,
-3.86890272396509));
#27968=CARTESIAN_POINT('Ctrl Pts',(-0.169540505433421,0.259978679799183,
-3.86360752882359));
#27969=CARTESIAN_POINT('Ctrl Pts',(-0.250158369544369,0.183721760385306,
-3.85831233368208));
#27970=CARTESIAN_POINT('Ctrl Pts',(-0.280264795244433,0.0910543401993367,
-3.85301713854058));
#27971=CARTESIAN_POINT('Ctrl Pts',(-0.289739918701928,0.0618899599604794,
-3.85135062959671));
#27972=CARTESIAN_POINT('Ctrl Pts',(-0.294211920145012,0.0311001313031377,
-3.84968412065283));
#27973=CARTESIAN_POINT('Ctrl Pts',(-0.29397219999165,0.000242578469533487,
-3.84801761170896));
#27974=CARTESIAN_POINT('Origin',(0.,0.,-4.78));
#27975=CARTESIAN_POINT('',(-0.29378381590831,-0.000139877028472651,-3.73358238829104));
#27976=CARTESIAN_POINT('',(-0.293811721941862,-0.000165168621852261,-3.74801761170896));
#27977=CARTESIAN_POINT('',(-0.2942,-3.60291088309151E-17,-4.78));
#27978=CARTESIAN_POINT('Ctrl Pts',(-0.29378381590831,-0.000139877028472651,
-3.73358238829104));
#27979=CARTESIAN_POINT('Ctrl Pts',(-0.293533849155245,0.0578968704636794,
-3.73671168180088));
#27980=CARTESIAN_POINT('Ctrl Pts',(-0.27691793885819,0.116065279437388,
-3.73984097531072));
#27981=CARTESIAN_POINT('Ctrl Pts',(-0.244888473326125,0.163916351090838,
-3.74297026882056));
#27982=CARTESIAN_POINT('Ctrl Pts',(-0.190690211086743,0.244886947597132,
-3.74826546396206));
#27983=CARTESIAN_POINT('Ctrl Pts',(-0.0923578601504312,0.296315606927623,
-3.75356065910357));
#27984=CARTESIAN_POINT('Ctrl Pts',(0.00506283766768875,0.294641572816598,
-3.75885585424507));
#27985=CARTESIAN_POINT('Ctrl Pts',(0.102483535485809,0.292967538705573,
-3.76415104938657));
#27986=CARTESIAN_POINT('Ctrl Pts',(0.198992580185736,0.238190811153031,
-3.76944624452807));
#27987=CARTESIAN_POINT('Ctrl Pts',(0.250376464661925,0.155405763325283,
-3.77474143966957));
#27988=CARTESIAN_POINT('Ctrl Pts',(0.301760349138113,0.0726207154975354,
-3.78003663481108));
#27989=CARTESIAN_POINT('Ctrl Pts',(0.308019073390562,-0.0381726526054187,
-3.78533182995258));
#27990=CARTESIAN_POINT('Ctrl Pts',(0.266285946015037,-0.126218084919271,
-3.79062702509408));
#27991=CARTESIAN_POINT('Ctrl Pts',(0.224552818639513,-0.214263517233121,
-3.79592222023558));
#27992=CARTESIAN_POINT('Ctrl Pts',(0.134827839636018,-0.279561013757871,
-3.80121741537709));
#27993=CARTESIAN_POINT('Ctrl Pts',(0.0382152982347072,-0.292196604806581,
-3.80651261051859));
#27994=CARTESIAN_POINT('Ctrl Pts',(-0.0583972431666067,-0.304832195855292,
-3.81180780566009));
#27995=CARTESIAN_POINT('Ctrl Pts',(-0.161897346965737,-0.264805881427962,
-3.81710300080159));
#27996=CARTESIAN_POINT('Ctrl Pts',(-0.224869677668475,-0.190454438241872,
-3.8223981959431));
#27997=CARTESIAN_POINT('Ctrl Pts',(-0.26920513275918,-0.138107557738643,
-3.82612626005908));
#27998=CARTESIAN_POINT('Ctrl Pts',(-0.293451716042893,-0.068746342158254,
-3.82985432417506));
#27999=CARTESIAN_POINT('Ctrl Pts',(-0.29402112681354,0.000254531718302781,
-3.83358238829104));
#28000=CARTESIAN_POINT('Ctrl Pts',(-0.29397219999165,0.000242578469533487,
-3.84801761170896));
#28001=CARTESIAN_POINT('Ctrl Pts',(-0.293450229068545,-0.0669472055825752,
-3.84438892551133));
#28002=CARTESIAN_POINT('Ctrl Pts',(-0.270589287922796,-0.134458079989008,
-3.84076023931371));
#28003=CARTESIAN_POINT('Ctrl Pts',(-0.228397637201052,-0.186208940374743,
-3.83713155311608));
#28004=CARTESIAN_POINT('Ctrl Pts',(-0.166829066168424,-0.261726879804802,
-3.83183635797458));
#28005=CARTESIAN_POINT('Ctrl Pts',(-0.0640969368139846,-0.303684837706857,
-3.82654116283307));
#28006=CARTESIAN_POINT('Ctrl Pts',(0.0327353628682028,-0.292861139192928,
-3.82124596769157));
#28007=CARTESIAN_POINT('Ctrl Pts',(0.12956766255039,-0.282037440678999,
-3.81595077255007));
#28008=CARTESIAN_POINT('Ctrl Pts',(0.220500132560325,-0.218432085749086,
-3.81065557740857));
#28009=CARTESIAN_POINT('Ctrl Pts',(0.263875069310696,-0.131183803754455,
-3.80536038226706));
#28010=CARTESIAN_POINT('Ctrl Pts',(0.307250006061066,-0.0439355217598243,
-3.80006518712556));
#28011=CARTESIAN_POINT('Ctrl Pts',(0.303067409551872,0.0669556872995245,
-3.79476999198406));
#28012=CARTESIAN_POINT('Ctrl Pts',(0.253243328461185,0.150688665578043,
-3.78947479684256));
#28013=CARTESIAN_POINT('Ctrl Pts',(0.203419247370498,0.234421643856562,
-3.78417960170105));
#28014=CARTESIAN_POINT('Ctrl Pts',(0.107953681698318,0.290996391354251,
-3.77888440655955));
#28015=CARTESIAN_POINT('Ctrl Pts',(0.0105811993363878,0.294494983786205,
-3.77358921141805));
#28016=CARTESIAN_POINT('Ctrl Pts',(-0.08679128302554,0.297993576218159,
-3.76829401627655));
#28017=CARTESIAN_POINT('Ctrl Pts',(-0.186070682077219,0.248416013584381,
-3.76299882113504));
#28018=CARTESIAN_POINT('Ctrl Pts',(-0.241775650694887,0.168474736970626,
-3.75770362599354));
#28019=CARTESIAN_POINT('Ctrl Pts',(-0.275740978842037,0.11973165785098,
-3.75447495456535));
#28020=CARTESIAN_POINT('Ctrl Pts',(-0.29350628959498,0.0597000159267478,
-3.75124628313715));
#28021=CARTESIAN_POINT('Ctrl Pts',(-0.293811721941862,-0.000165168621852261,
-3.74801761170896));
#28022=CARTESIAN_POINT('Origin',(0.,0.,-4.78));
#28023=CARTESIAN_POINT('',(-0.294602820716591,-0.000172945526623114,-3.63358238829104));
#28024=CARTESIAN_POINT('',(-0.294584692827634,-0.000157098441292656,-3.64801761170896));
#28025=CARTESIAN_POINT('',(-0.2942,-3.60291088309151E-17,-4.78));
#28026=CARTESIAN_POINT('Ctrl Pts',(-0.294602820716591,-0.000172945526623114,
-3.63358238829104));
#28027=CARTESIAN_POINT('Ctrl Pts',(-0.293985296127081,0.0862757997737715,
-3.6382738442852));
#28028=CARTESIAN_POINT('Ctrl Pts',(-0.253543207095474,0.173218312496561,
-3.64296530027936));
#28029=CARTESIAN_POINT('Ctrl Pts',(-0.186746316274069,0.227928150582927,
-3.64765675627352));
#28030=CARTESIAN_POINT('Ctrl Pts',(-0.111353395145683,0.289678547301548,
-3.65295195141502));
#28031=CARTESIAN_POINT('Ctrl Pts',(-0.00238606325056179,0.310366481589784,
-3.65824714655652));
#28032=CARTESIAN_POINT('Ctrl Pts',(0.0903415413845116,0.280493415878642,
-3.66354234169803));
#28033=CARTESIAN_POINT('Ctrl Pts',(0.183069146019585,0.2506203501675,-3.66883753683953));
#28034=CARTESIAN_POINT('Ctrl Pts',(0.259557023394611,0.17018628445698,-3.67413273198103));
#28035=CARTESIAN_POINT('Ctrl Pts',(0.284710385565443,0.0760501837047467,
-3.67942792712253));
#28036=CARTESIAN_POINT('Ctrl Pts',(0.309863747736276,-0.0180859170474864,
-3.68472312226404));
#28037=CARTESIAN_POINT('Ctrl Pts',(0.283682594702916,-0.125924052841432,
-3.69001831740554));
#28038=CARTESIAN_POINT('Ctrl Pts',(0.218189061309932,-0.198067237438836,
-3.69531351254704));
#28039=CARTESIAN_POINT('Ctrl Pts',(0.152695527916949,-0.27021042203624,
-3.70060870768854));
#28040=CARTESIAN_POINT('Ctrl Pts',(0.0478896141643412,-0.306658655437101,
-3.70590390283004));
#28041=CARTESIAN_POINT('Ctrl Pts',(-0.0482298065556536,-0.290711509461145,
-3.71119909797155));
#28042=CARTESIAN_POINT('Ctrl Pts',(-0.144349227275646,-0.274764363485189,
-3.71649429311305));
#28043=CARTESIAN_POINT('Ctrl Pts',(-0.231782154963025,-0.206421838132418,
-3.72178948825455));
#28044=CARTESIAN_POINT('Ctrl Pts',(-0.270466532035491,-0.116994308614986,
-3.72708468339606));
#28045=CARTESIAN_POINT('Ctrl Pts',(-0.286289660963147,-0.0804156317350293,
-3.72925058502772));
#28046=CARTESIAN_POINT('Ctrl Pts',(-0.29395682729143,-0.040309290889572,
-3.73141648665938));
#28047=CARTESIAN_POINT('Ctrl Pts',(-0.29378381590831,-0.000139877028472651,
-3.73358238829104));
#28048=CARTESIAN_POINT('Ctrl Pts',(-0.293811721941862,-0.000165168621852261,
-3.74801761170896));
#28049=CARTESIAN_POINT('Ctrl Pts',(-0.294007215104199,-0.0384821129819785,
-3.74595108799565));
#28050=CARTESIAN_POINT('Ctrl Pts',(-0.287049937609616,-0.0767308649180593,
-3.74388456428235));
#28051=CARTESIAN_POINT('Ctrl Pts',(-0.272609541015007,-0.111907800977432,
-3.74181804056904));
#28052=CARTESIAN_POINT('Ctrl Pts',(-0.235607924533802,-0.202044071717994,
-3.73652284542754));
#28053=CARTESIAN_POINT('Ctrl Pts',(-0.149474153387738,-0.27201162260538,
-3.73122765028603));
#28054=CARTESIAN_POINT('Ctrl Pts',(-0.0536685951641096,-0.289756730929934,
-3.72593245514453));
#28055=CARTESIAN_POINT('Ctrl Pts',(0.0421369630595187,-0.307501839254488,
-3.72063726000303));
#28056=CARTESIAN_POINT('Ctrl Pts',(0.147614308360711,-0.27302450501621,
-3.71534206486152));
#28057=CARTESIAN_POINT('Ctrl Pts',(0.214444362295811,-0.20212011735872,
-3.71004686972002));
#28058=CARTESIAN_POINT('Ctrl Pts',(0.28127441623091,-0.131215729701233,
-3.70475167457852));
#28059=CARTESIAN_POINT('Ctrl Pts',(0.309457178799918,-0.023884288624536,
-3.69945647943702));
#28060=CARTESIAN_POINT('Ctrl Pts',(0.286077924579446,0.0707052133088147,
-3.69416128429552));
#28061=CARTESIAN_POINT('Ctrl Pts',(0.262698670358975,0.165294715242165,
-3.68886608915401));
#28062=CARTESIAN_POINT('Ctrl Pts',(0.187757399349022,0.24714227803217,-3.68357089401251));
#28063=CARTESIAN_POINT('Ctrl Pts',(0.0955931833176489,0.278749407497395,
-3.67827569887101));
#28064=CARTESIAN_POINT('Ctrl Pts',(0.00342896728627082,0.310356536962622,
-3.6729805037295));
#28065=CARTESIAN_POINT('Ctrl Pts',(-0.105958193766529,0.291723233103062,
-3.667685308588));
#28066=CARTESIAN_POINT('Ctrl Pts',(-0.182470015924895,0.231390967676254,
-3.6623901134465));
#28067=CARTESIAN_POINT('Ctrl Pts',(-0.251694175282413,0.17680528093544,
-3.65759927953399));
#28068=CARTESIAN_POINT('Ctrl Pts',(-0.294007415616088,0.0880858813310743,
-3.65280844562147));
#28069=CARTESIAN_POINT('Ctrl Pts',(-0.294584692827634,-0.000157098441292656,
-3.64801761170896));
#28070=CARTESIAN_POINT('Origin',(0.,0.,-6.1506589891905));
#28071=CARTESIAN_POINT('',(-0.237499741684084,-0.000139423369390631,-3.6006589891905));
#28072=CARTESIAN_POINT('',(-0.237175,1.98931295048561E-15,-3.6));
#28073=CARTESIAN_POINT('',(-0.237175,1.98931295048561E-15,-6.1506589891905));
#28074=CARTESIAN_POINT('',(-0.236971720686989,-0.00981754651873418,-3.6));
#28075=CARTESIAN_POINT('Ctrl Pts',(-0.237499741684084,-0.000139423369390674,
-3.6006589891905));
#28076=CARTESIAN_POINT('Ctrl Pts',(-0.237523051019196,-0.00340255298153232,
-3.600439326127));
#28077=CARTESIAN_POINT('Ctrl Pts',(-0.237475976012487,-0.00666480992888717,
-3.6002196630635));
#28078=CARTESIAN_POINT('Ctrl Pts',(-0.237357402024655,-0.00992348605843001,
-3.6));
#28079=CARTESIAN_POINT('Origin',(0.,0.,-3.6));
#28080=CARTESIAN_POINT('Origin',(0.,0.,-6.1506589891905));
#28081=CARTESIAN_POINT('',(-0.236839485173533,-0.000112764562290553,-3.7006589891905));
#28082=CARTESIAN_POINT('',(-0.237485127537029,-0.000126647936150415,-3.6809410108095));
#28083=CARTESIAN_POINT('',(-0.237175,1.98931295048561E-15,-6.1506589891905));
#28084=CARTESIAN_POINT('Ctrl Pts',(-0.236839485173533,-0.000112764562290573,
-3.7006589891905));
#28085=CARTESIAN_POINT('Ctrl Pts',(-0.236978961634416,-0.0324961117156111,
-3.69849308755884));
#28086=CARTESIAN_POINT('Ctrl Pts',(-0.215686539381533,-0.143875088998195,
-3.69103199078568));
#28087=CARTESIAN_POINT('Ctrl Pts',(-0.0458841718383633,-0.276602230999808,
-3.67827569887101));
#28088=CARTESIAN_POINT('Ctrl Pts',(0.207589749925143,-0.188451893574426,
-3.6623901134465));
#28089=CARTESIAN_POINT('Ctrl Pts',(0.27090907321563,0.0723554809013986,
-3.64650452802199));
#28090=CARTESIAN_POINT('Ctrl Pts',(0.0859225438163616,0.266885897640616,
-3.63061894259749));
#28091=CARTESIAN_POINT('Ctrl Pts',(-0.167599901511316,0.218753529908791,
-3.61533709632032));
#28092=CARTESIAN_POINT('Ctrl Pts',(-0.237001912334942,0.0695528987469263,
-3.60535044518466));
#28093=CARTESIAN_POINT('Ctrl Pts',(-0.237499741684084,-0.000139423369390674,
-3.6006589891905));
#28094=CARTESIAN_POINT('',(-0.0864920085589077,0.220841828194855,-3.6));
#28095=CARTESIAN_POINT('Origin',(0.,0.,-3.6));
#28096=CARTESIAN_POINT('Ctrl Pts',(-0.237485127537029,-0.000126647936150416,
-3.6809410108095));
#28097=CARTESIAN_POINT('Ctrl Pts',(-0.237534121349303,-0.00761587477375465,
-3.68043664958051));
#28098=CARTESIAN_POINT('Ctrl Pts',(-0.233809530212368,-0.093684159787474,
-3.67463709321002));
#28099=CARTESIAN_POINT('Ctrl Pts',(-0.12883195646667,-0.249024285245638,
-3.66354234169802));
#28100=CARTESIAN_POINT('Ctrl Pts',(0.139350939164339,-0.243214763219636,
-3.64765675627352));
#28101=CARTESIAN_POINT('Ctrl Pts',(0.280177793680504,-0.0146860234836151,
-3.63177117084901));
#28102=CARTESIAN_POINT('Ctrl Pts',(0.163650290907218,0.227552512000709,
-3.61588558542451));
#28103=CARTESIAN_POINT('Ctrl Pts',(-0.0130164034045845,0.24961831823673,
-3.6052951951415));
#28104=CARTESIAN_POINT('Ctrl Pts',(-0.0864920085589077,0.220841828194855,
-3.6));
#28105=CARTESIAN_POINT('Origin',(0.,0.,-6.1506589891905));
#28106=CARTESIAN_POINT('',(-0.237030797933384,0.000205195650219347,-3.8006589891905));
#28107=CARTESIAN_POINT('',(-0.236861982160303,-0.000133153867742014,-3.7809410108095));
#28108=CARTESIAN_POINT('',(-0.237175,1.98931295048561E-15,-6.1506589891905));
#28109=CARTESIAN_POINT('Ctrl Pts',(-0.237030797933384,0.000205195650219349,
-3.8006589891905));
#28110=CARTESIAN_POINT('Ctrl Pts',(-0.236571756466603,-0.0554211886518688,
-3.79693092507452));
#28111=CARTESIAN_POINT('Ctrl Pts',(-0.189261331157349,-0.190760199954121,
-3.78790766581703));
#28112=CARTESIAN_POINT('Ctrl Pts',(0.0363605403484637,-0.278014334385727,
-3.77358921141805));
#28113=CARTESIAN_POINT('Ctrl Pts',(0.253361103521349,-0.12009182855713,
-3.75770362599354));
#28114=CARTESIAN_POINT('Ctrl Pts',(0.238224329987279,0.147862798361475,
-3.74181804056903));
#28115=CARTESIAN_POINT('Ctrl Pts',(0.00481645089103148,0.280340742181402,
-3.72593245514453));
#28116=CARTESIAN_POINT('Ctrl Pts',(-0.200576150596734,0.17291865748255,
-3.71221277135168));
#28117=CARTESIAN_POINT('Ctrl Pts',(-0.236637969658038,0.0466746779477384,
-3.70378828270034));
#28118=CARTESIAN_POINT('Ctrl Pts',(-0.236839485173533,-0.000112764562290573,
-3.7006589891905));
#28119=CARTESIAN_POINT('Ctrl Pts',(-0.236861982160303,-0.000133153867742007,
-3.7809410108095));
#28120=CARTESIAN_POINT('Ctrl Pts',(-0.237019582740782,-0.0310230970309381,
-3.77887448709619));
#28121=CARTESIAN_POINT('Ctrl Pts',(-0.217039172494002,-0.140868615727758,
-3.77151276824138));
#28122=CARTESIAN_POINT('Ctrl Pts',(-0.0510630698782088,-0.275693101540268,
-3.75885585424507));
#28123=CARTESIAN_POINT('Ctrl Pts',(0.204034714334676,-0.192309399147709,
-3.74297026882056));
#28124=CARTESIAN_POINT('Ctrl Pts',(0.272194945935335,0.0672725301932114,
-3.72708468339606));
#28125=CARTESIAN_POINT('Ctrl Pts',(0.0909488961210605,0.265221500669614,
-3.71119909797155));
#28126=CARTESIAN_POINT('Ctrl Pts',(-0.165205329670506,0.221587499401578,
-3.69581787377603));
#28127=CARTESIAN_POINT('Ctrl Pts',(-0.237019744387309,0.0710121308793213,
-3.68573184472201));
#28128=CARTESIAN_POINT('Ctrl Pts',(-0.237485127537029,-0.000126647936150416,
-3.6809410108095));
#28129=CARTESIAN_POINT('Origin',(0.,0.,-6.1506589891905));
#28130=CARTESIAN_POINT('',(-0.237565997280583,1.38059634504043E-6,-3.9006589891905));
#28131=CARTESIAN_POINT('',(-0.236991354632969,0.000195559308326751,-3.8809410108095));
#28132=CARTESIAN_POINT('',(-0.237175,1.98931295048561E-15,-6.1506589891905));
#28133=CARTESIAN_POINT('Ctrl Pts',(-0.237565992246873,1.38057857121606E-6,
-3.9006589891905));
#28134=CARTESIAN_POINT('Ctrl Pts',(-0.237559231926505,-0.0784743142974118,
-3.8953687625902));
#28135=CARTESIAN_POINT('Ctrl Pts',(-0.152071038566501,-0.235512023820444,
-3.8847833408484));
#28136=CARTESIAN_POINT('Ctrl Pts',(0.115481785178347,-0.255495584003526,
-3.86890272396509));
#28137=CARTESIAN_POINT('Ctrl Pts',(0.277309894480033,-0.0413914846015558,
-3.85301713854059));
#28138=CARTESIAN_POINT('Ctrl Pts',(0.185057083358657,0.210636924353684,
-3.83713155311608));
#28139=CARTESIAN_POINT('Ctrl Pts',(-0.0767514749289204,0.269672488584438,
-3.82124596769156));
#28140=CARTESIAN_POINT('Ctrl Pts',(-0.223299221161425,0.125756213525167,
-3.80908844638305));
#28141=CARTESIAN_POINT('Ctrl Pts',(-0.23722376084985,0.023588332303802,
-3.80222612021602));
#28142=CARTESIAN_POINT('Ctrl Pts',(-0.237030797933384,0.000205195650219349,
-3.8006589891905));
#28143=CARTESIAN_POINT('Ctrl Pts',(-0.236991354632969,0.000195559308326754,
-3.8809410108095));
#28144=CARTESIAN_POINT('Ctrl Pts',(-0.236570557713568,-0.0539707800273571,
-3.87731232461187));
#28145=CARTESIAN_POINT('Ctrl Pts',(-0.191246924065396,-0.187816456780419,
-3.86838844327274));
#28146=CARTESIAN_POINT('Ctrl Pts',(0.0311465050672407,-0.278646601116737,
-3.85416936679211));
#28147=CARTESIAN_POINT('Ctrl Pts',(0.251067394679135,-0.124816552964098,
-3.83828378136761));
#28148=CARTESIAN_POINT('Ctrl Pts',(0.240951752322899,0.143374703072453,
-3.82239819594309));
#28149=CARTESIAN_POINT('Ctrl Pts',(0.0100675354129855,0.280201172186297,
-3.80651261051859));
#28150=CARTESIAN_POINT('Ctrl Pts',(-0.198805302366879,0.175895482421437,
-3.79269354880739));
#28151=CARTESIAN_POINT('Ctrl Pts',(-0.236615751987389,0.0481283184140897,
-3.78416968223769));
#28152=CARTESIAN_POINT('Ctrl Pts',(-0.236861982160303,-0.000133153867742007,
-3.7809410108095));
#28153=CARTESIAN_POINT('Origin',(0.,0.,-6.1506589891905));
#28154=CARTESIAN_POINT('',(-0.237034860401358,-0.000206013329817485,-4.0006589891905));
#28155=CARTESIAN_POINT('',(-0.237561645443886,2.88892589412493E-5,-3.9809410108095));
#28156=CARTESIAN_POINT('',(-0.237175,1.98931295048561E-15,-6.1506589891905));
#28157=CARTESIAN_POINT('Ctrl Pts',(-0.237034860401358,-0.000206013329817466,
-4.0006589891905));
#28158=CARTESIAN_POINT('Ctrl Pts',(-0.237227612547211,-0.0234398712075855,
-3.99910179524738));
#28159=CARTESIAN_POINT('Ctrl Pts',(-0.22341484328665,-0.125455592362394,
-3.99224940616276));
#28160=CARTESIAN_POINT('Ctrl Pts',(-0.0772564444343335,-0.269528249207591,
-3.98010182193664));
#28161=CARTESIAN_POINT('Ctrl Pts',(0.184662206520241,-0.210983186133545,
-3.96421623651213));
#28162=CARTESIAN_POINT('Ctrl Pts',(0.277386942916036,0.0408719852250892,
-3.94833065108763));
#28163=CARTESIAN_POINT('Ctrl Pts',(0.115960147730902,0.25527882694822,-3.93244506566312));
#28164=CARTESIAN_POINT('Ctrl Pts',(-0.151713354856548,0.235790359050968,
-3.91655948023861));
#28165=CARTESIAN_POINT('Ctrl Pts',(-0.237532576511483,0.0786981808764117,
-3.9059641214144));
#28166=CARTESIAN_POINT('Ctrl Pts',(-0.237565998596115,7.50843634444512E-5,
-3.9006639577317));
#28167=CARTESIAN_POINT('Ctrl Pts',(-0.237565992246873,1.38057857121606E-6,
-3.9006589891905));
#28168=CARTESIAN_POINT('Ctrl Pts',(-0.237561645443886,2.88892589412437E-5,
-3.9809410108095));
#28169=CARTESIAN_POINT('Ctrl Pts',(-0.237429395637666,-0.0769764098845311,
-3.97575016212755));
#28170=CARTESIAN_POINT('Ctrl Pts',(-0.154784114476735,-0.232778614358938,
-3.9652641183041));
#28171=CARTESIAN_POINT('Ctrl Pts',(0.110675778439994,-0.257613859497429,
-3.94948287933915));
#28172=CARTESIAN_POINT('Ctrl Pts',(0.276485921807596,-0.0465785687612247,
-3.93359729391465));
#28173=CARTESIAN_POINT('Ctrl Pts',(0.188970082294562,0.207133620332956,
-3.91771170849014));
#28174=CARTESIAN_POINT('Ctrl Pts',(-0.0716867010729343,0.271062808441053,
-3.90182612306563));
#28175=CARTESIAN_POINT('Ctrl Pts',(-0.222124224235629,0.128763056306054,
-3.88956922383875));
#28176=CARTESIAN_POINT('Ctrl Pts',(-0.237184609654634,0.025071970230525,
-3.88260751975337));
#28177=CARTESIAN_POINT('Ctrl Pts',(-0.236991354632969,0.000195559308326754,
-3.8809410108095));
#28178=CARTESIAN_POINT('Origin',(0.,0.,-6.1506589891905));
#28179=CARTESIAN_POINT('',(-0.236836491818845,0.000110831649961404,-4.1006589891905));
#28180=CARTESIAN_POINT('',(-0.237076567927639,-0.000212689822428169,-4.0809410108095));
#28181=CARTESIAN_POINT('',(-0.237175,1.98931295048561E-15,-6.1506589891905));
#28182=CARTESIAN_POINT('Ctrl Pts',(-0.236836491818845,0.000110831649961389,
-4.1006589891905));
#28183=CARTESIAN_POINT('Ctrl Pts',(-0.236639836850206,-0.0465291493340525,
-4.09753963276306));
#28184=CARTESIAN_POINT('Ctrl Pts',(-0.200752511647945,-0.172621020014775,
-4.08912508119413));
#28185=CARTESIAN_POINT('Ctrl Pts',(0.00429227712398719,-0.280349088964778,
-4.07541533448367));
#28186=CARTESIAN_POINT('Ctrl Pts',(0.237946464991633,-0.148308850460187,
-4.05952974905918));
#28187=CARTESIAN_POINT('Ctrl Pts',(0.253585853911662,0.11961709752968,-4.04364416363466));
#28188=CARTESIAN_POINT('Ctrl Pts',(0.0368810936713182,0.2779457145844,-4.02775857821017));
#28189=CARTESIAN_POINT('Ctrl Pts',(-0.189060335164718,0.191054117653322,
-4.01343018672877));
#28190=CARTESIAN_POINT('Ctrl Pts',(-0.23657216418078,0.0555662229892069,
-4.00439699038888));
#28191=CARTESIAN_POINT('Ctrl Pts',(-0.237034860401358,-0.000206013329817466,
-4.0006589891905));
#28192=CARTESIAN_POINT('Ctrl Pts',(-0.237076567927639,-0.000212689822428173,
-4.0809410108095));
#28193=CARTESIAN_POINT('Ctrl Pts',(-0.237265375825923,-0.0219540932160755,
-4.07948319478473));
#28194=CARTESIAN_POINT('Ctrl Pts',(-0.224552153366904,-0.122449579388927,
-4.07273018361847));
#28195=CARTESIAN_POINT('Ctrl Pts',(-0.0822914743374018,-0.268033844229383,
-4.0606819773107));
#28196=CARTESIAN_POINT('Ctrl Pts',(0.180677832160775,-0.214405105746405,
-4.04479639188619));
#28197=CARTESIAN_POINT('Ctrl Pts',(0.278103846141642,0.0356690223564828,
-4.02891080646169));
#28198=CARTESIAN_POINT('Ctrl Pts',(0.1207214766735,0.253061955797574,-4.01302522103717));
#28199=CARTESIAN_POINT('Ctrl Pts',(-0.14727009426389,0.238590753715125,
-3.99713963561268));
#28200=CARTESIAN_POINT('Ctrl Pts',(-0.236849170311852,0.081675548847311,
-3.98644489887011));
#28201=CARTESIAN_POINT('Ctrl Pts',(-0.237564303929984,0.00157685006938821,
-3.98104535726905));
#28202=CARTESIAN_POINT('Ctrl Pts',(-0.237561645443886,2.88892589412437E-5,
-3.9809410108095));
#28203=CARTESIAN_POINT('Origin',(0.,0.,-6.1506589891905));
#28204=CARTESIAN_POINT('',(-0.237440599831179,0.000151834494169013,-4.2006589891905));
#28205=CARTESIAN_POINT('',(-0.236817680733397,8.90465815239633E-5,-4.1809410108095));
#28206=CARTESIAN_POINT('',(-0.237175,1.98931295048561E-15,-6.1506589891905));
#28207=CARTESIAN_POINT('Ctrl Pts',(-0.237440599831179,0.000151834494169018,
-4.2006589891905));
#28208=CARTESIAN_POINT('Ctrl Pts',(-0.236922564689605,-0.0693914648962057,
-4.19597747027874));
#28209=CARTESIAN_POINT('Ctrl Pts',(-0.167933984931827,-0.218488341387412,
-4.18600075622548));
#28210=CARTESIAN_POINT('Ctrl Pts',(0.0854715091573248,-0.267036807292018,
-4.17072884703072));
#28211=CARTESIAN_POINT('Ctrl Pts',(0.270747721571937,-0.0728677335311189,
-4.15484326160622));
#28212=CARTESIAN_POINT('Ctrl Pts',(0.207955486803503,0.188065283438102,
-4.1389576761817));
#28213=CARTESIAN_POINT('Ctrl Pts',(-0.0453727731435854,0.276686368987695,
-4.12307209075721));
#28214=CARTESIAN_POINT('Ctrl Pts',(-0.215547649412793,0.144175982261373,
-4.11030586176013));
#28215=CARTESIAN_POINT('Ctrl Pts',(-0.23697366418245,0.0326435282522547,
-4.10283482790456));
#28216=CARTESIAN_POINT('Ctrl Pts',(-0.236836491818845,0.000110831649961389,
-4.1006589891905));
#28217=CARTESIAN_POINT('Ctrl Pts',(-0.236817680733397,8.90465815239772E-5,
-4.1809410108095));
#28218=CARTESIAN_POINT('Ctrl Pts',(-0.236665414212453,-0.0450740145522511,
-4.17792103230042));
#28219=CARTESIAN_POINT('Ctrl Pts',(-0.202479259262566,-0.169638983975812,
-4.16960585864983));
#28220=CARTESIAN_POINT('Ctrl Pts',(-0.000959750965527487,-0.280380290461363,
-4.15599548985773));
#28221=CARTESIAN_POINT('Ctrl Pts',(0.235126705419149,-0.152739846798193,
-4.14010990443324));
#28222=CARTESIAN_POINT('Ctrl Pts',(0.255781924318054,0.114846138782203,
-4.12422431900872));
#28223=CARTESIAN_POINT('Ctrl Pts',(0.0420808782244523,0.277206111204153,
-4.10833873358422));
#28224=CARTESIAN_POINT('Ctrl Pts',(-0.187026567625837,0.193988718634259,
-4.09391096418447));
#28225=CARTESIAN_POINT('Ctrl Pts',(-0.236579572783091,0.0570167588419758,
-4.08477838992624));
#28226=CARTESIAN_POINT('Ctrl Pts',(-0.237076567927639,-0.000212689822428173,
-4.0809410108095));
#28227=CARTESIAN_POINT('Origin',(0.,0.,-6.1506589891905));
#28228=CARTESIAN_POINT('',(-0.237304285819382,-0.000201120099325924,-4.3006589891905));
#28229=CARTESIAN_POINT('',(-0.237403111349647,0.000169659163617816,-4.2809410108095));
#28230=CARTESIAN_POINT('',(-0.237175,1.98931295048561E-15,-6.1506589891905));
#28231=CARTESIAN_POINT('Ctrl Pts',(-0.237304285819382,-0.000201120099325937,
-4.3006589891905));
#28232=CARTESIAN_POINT('Ctrl Pts',(-0.237431694732867,-0.0143118172002052,
-4.29971050293593));
#28233=CARTESIAN_POINT('Ctrl Pts',(-0.229859658596377,-0.107062981526376,
-4.29346682153985));
#28234=CARTESIAN_POINT('Ctrl Pts',(-0.107605972147853,-0.258911162533527,
-4.28192794500227));
#28235=CARTESIAN_POINT('Ctrl Pts',(0.159293148852347,-0.230737357302738,
-4.26604235957777));
#28236=CARTESIAN_POINT('Ctrl Pts',(0.2802423654424,0.00884601252520937,
-4.25015677415325));
#28237=CARTESIAN_POINT('Ctrl Pts',(0.144423813031258,0.240324359056379,
-4.23427118872875));
#28238=CARTESIAN_POINT('Ctrl Pts',(-0.123720842908662,0.251609197678298,
-4.21838560330425));
#28239=CARTESIAN_POINT('Ctrl Pts',(-0.232891988211843,0.096973930455177,
-4.20718153679149));
#28240=CARTESIAN_POINT('Ctrl Pts',(-0.23750850639282,0.0092679078409494,
-4.20127266542025));
#28241=CARTESIAN_POINT('Ctrl Pts',(-0.237440599831179,0.000151834494169018,
-4.2006589891905));
#28242=CARTESIAN_POINT('Ctrl Pts',(-0.237403111349647,0.000169659163617811,
-4.28094101080949));
#28243=CARTESIAN_POINT('Ctrl Pts',(-0.236852466100401,-0.0679255050907547,
-4.27635886981609));
#28244=CARTESIAN_POINT('Ctrl Pts',(-0.170354300778626,-0.21565114223581,
-4.26648153368119));
#28245=CARTESIAN_POINT('Ctrl Pts',(0.0804545900663122,-0.268590929367298,
-4.25130900240478));
#28246=CARTESIAN_POINT('Ctrl Pts',(0.269335308407912,-0.0779263758039853,
-4.23542341698027));
#28247=CARTESIAN_POINT('Ctrl Pts',(0.211441681464576,0.184137024361096,
-4.21953783155577));
#28248=CARTESIAN_POINT('Ctrl Pts',(-0.0401821430447466,0.277487700234545,
-4.20365224613126));
#28249=CARTESIAN_POINT('Ctrl Pts',(-0.214153039044315,0.14718162281968,
-4.19078663921584));
#28250=CARTESIAN_POINT('Ctrl Pts',(-0.236932396556695,0.0341143707861283,
-4.18321622744192));
#28251=CARTESIAN_POINT('Ctrl Pts',(-0.236817680733397,8.90465815239772E-5,
-4.1809410108095));
#28252=CARTESIAN_POINT('Origin',(0.,0.,-6.1506589891905));
#28253=CARTESIAN_POINT('',(-0.236790373551236,-3.35771274733464E-5,-4.4006589891905));
#28254=CARTESIAN_POINT('',(-0.23734735502029,-0.000189769014714958,-4.38094101080949));
#28255=CARTESIAN_POINT('',(-0.237175,1.98931295048561E-15,-6.1506589891905));
#28256=CARTESIAN_POINT('Ctrl Pts',(-0.236790373551236,-3.35771274733478E-5,
-4.4006589891905));
#28257=CARTESIAN_POINT('Ctrl Pts',(-0.236837795918825,-0.0375905476484022,
-4.39814834045161));
#28258=CARTESIAN_POINT('Ctrl Pts',(-0.210698941147542,-0.154296333752042,
-4.39034249657121));
#28259=CARTESIAN_POINT('Ctrl Pts',(-0.0278323017717629,-0.27899712956307,
-4.37724145754931));
#28260=CARTESIAN_POINT('Ctrl Pts',(0.219402452553475,-0.174575482642516,
-4.36135587212481));
#28261=CARTESIAN_POINT('Ctrl Pts',(0.265613074904189,0.0897982726241923,
-4.3454702867003));
#28262=CARTESIAN_POINT('Ctrl Pts',(0.0684597913264363,0.271895737917843,
-4.32958470127579));
#28263=CARTESIAN_POINT('Ctrl Pts',(-0.1759020676831,0.20887465967552,-4.31464760210586));
#28264=CARTESIAN_POINT('Ctrl Pts',(-0.23672039812059,0.0644651754777562,
-4.30500569807743));
#28265=CARTESIAN_POINT('Ctrl Pts',(-0.237304285819382,-0.000201120099325937,
-4.3006589891905));
#28266=CARTESIAN_POINT('Ctrl Pts',(-0.23734735502029,-0.000189769014714986,
-4.38094101080949));
#28267=CARTESIAN_POINT('Ctrl Pts',(-0.237457523554163,-0.0128160771384688,
-4.38009190247327));
#28268=CARTESIAN_POINT('Ctrl Pts',(-0.230796517221853,-0.104065922452244,
-4.37394759899555));
#28269=CARTESIAN_POINT('Ctrl Pts',(-0.112436805309618,-0.256850137654031,
-4.36250810037634));
#28270=CARTESIAN_POINT('Ctrl Pts',(0.154943207178462,-0.23368061740414,
-4.34662251495182));
#28271=CARTESIAN_POINT('Ctrl Pts',(0.280358882596026,0.00359518436732559,
-4.33073692952732));
#28272=CARTESIAN_POINT('Ctrl Pts',(0.14890003195752,0.237576953604884,-4.3148513441028));
#28273=CARTESIAN_POINT('Ctrl Pts',(-0.11898618914506,0.253882483038636,
-4.29896575867831));
#28274=CARTESIAN_POINT('Ctrl Pts',(-0.232028528892651,0.0999660525608262,
-4.2876623142472));
#28275=CARTESIAN_POINT('Ctrl Pts',(-0.237488800524134,0.0107663517156311,
-4.28165406495759));
#28276=CARTESIAN_POINT('Ctrl Pts',(-0.237403111349647,0.000169659163617811,
-4.28094101080949));
#28277=CARTESIAN_POINT('Origin',(0.,0.,-6.1506589891905));
#28278=CARTESIAN_POINT('',(-0.237180885702784,0.000217072097893513,-4.5006589891905));
#28279=CARTESIAN_POINT('',(-0.236798869759374,-5.74984565626796E-5,-4.4809410108095));
#28280=CARTESIAN_POINT('',(-0.237175,1.98931295048561E-15,-6.1506589891905));
#28281=CARTESIAN_POINT('Ctrl Pts',(-0.237180885702784,0.000217072097893506,
-4.5006589891905));
#28282=CARTESIAN_POINT('Ctrl Pts',(-0.236621983925057,-0.0604554976673563,
-4.49658617796729));
#28283=CARTESIAN_POINT('Ctrl Pts',(-0.182031586694785,-0.200904114215803,
-4.48721817160257));
#28284=CARTESIAN_POINT('Ctrl Pts',(0.0543372398400151,-0.275066355072582,
-4.47255497009635));
#28285=CARTESIAN_POINT('Ctrl Pts',(0.260625067348198,-0.103385732072151,
-4.45666938467185));
#28286=CARTESIAN_POINT('Ctrl Pts',(0.228119174345422,0.163020482217144,
-4.44078379924733));
#28287=CARTESIAN_POINT('Ctrl Pts',(-0.0133974132773538,0.280061680070342,
-4.42489821382283));
#28288=CARTESIAN_POINT('Ctrl Pts',(-0.206408202951183,0.16255768074852,
-4.41152327713722));
#28289=CARTESIAN_POINT('Ctrl Pts',(-0.23673777766993,0.0416206477494621,
-4.40344353559311));
#28290=CARTESIAN_POINT('Ctrl Pts',(-0.236790373551236,-3.35771274733478E-5,
-4.4006589891905));
#28291=CARTESIAN_POINT('Ctrl Pts',(-0.236798869759374,-5.74984565626727E-5,
-4.4809410108095));
#28292=CARTESIAN_POINT('Ctrl Pts',(-0.236877019742237,-0.0361246334101674,
-4.47852973998896));
#28293=CARTESIAN_POINT('Ctrl Pts',(-0.212182948306362,-0.151294347002612,
-4.47082327402691));
#28294=CARTESIAN_POINT('Ctrl Pts',(-0.0330533685498055,-0.278426836401662,
-4.45782161292337));
#28295=CARTESIAN_POINT('Ctrl Pts',(0.216093941700501,-0.178654517887089,
-4.44193602749886));
#28296=CARTESIAN_POINT('Ctrl Pts',(0.26724849229964,0.0848072624525569,
-4.42605044207435));
#28297=CARTESIAN_POINT('Ctrl Pts',(0.0735407108656338,0.270565689337182,
-4.41016485664985));
#28298=CARTESIAN_POINT('Ctrl Pts',(-0.173592056620874,0.211744102334454,
-4.39512837956156));
#28299=CARTESIAN_POINT('Ctrl Pts',(-0.236770492394035,0.0659238934636766,
-4.38538709761478));
#28300=CARTESIAN_POINT('Ctrl Pts',(-0.23734735502029,-0.000189769014714986,
-4.38094101080949));
#28301=CARTESIAN_POINT('Origin',(0.,0.,-6.1506589891905));
#28302=CARTESIAN_POINT('',(-0.237523476840667,-9.09874636312175E-5,-4.6006589891905));
#28303=CARTESIAN_POINT('',(-0.237136177256987,0.000217231692762283,-4.5809410108095));
#28304=CARTESIAN_POINT('',(-0.237175,1.98931295048561E-15,-6.1506589891905));
#28305=CARTESIAN_POINT('Ctrl Pts',(-0.237523476840667,-9.09874636312079E-5,
-4.6006589891905));
#28306=CARTESIAN_POINT('Ctrl Pts',(-0.237548180986008,-0.00513370532888432,
-4.60031921062447));
#28307=CARTESIAN_POINT('Ctrl Pts',(-0.235115874964421,-0.0887391407442366,
-4.59468423691694));
#28308=CARTESIAN_POINT('Ctrl Pts',(-0.13654042413847,-0.244889256404674,
-4.5837540680679));
#28309=CARTESIAN_POINT('Ctrl Pts',(0.131829301628996,-0.247457209550174,
-4.56786848264339));
#28310=CARTESIAN_POINT('Ctrl Pts',(0.279412451766375,-0.0232962899245847,
-4.55198289721889));
#28311=CARTESIAN_POINT('Ctrl Pts',(0.170988228579068,0.222209498027739,
-4.53609731179438));
#28312=CARTESIAN_POINT('Ctrl Pts',(-0.0941013364397791,0.264119241643986,
-4.52021172636988));
#28313=CARTESIAN_POINT('Ctrl Pts',(-0.227112405750096,0.115332508093694,
-4.50839895216858));
#28314=CARTESIAN_POINT('Ctrl Pts',(-0.237348630414619,0.0184268956074038,
-4.50188137310879));
#28315=CARTESIAN_POINT('Ctrl Pts',(-0.237180885702784,0.000217072097893506,
-4.5006589891905));
#28316=CARTESIAN_POINT('Ctrl Pts',(-0.237136177256987,0.000217231692762269,
-4.5809410108095));
#28317=CARTESIAN_POINT('Ctrl Pts',(-0.236599623077143,-0.0590033993122846,
-4.57696757750464));
#28318=CARTESIAN_POINT('Ctrl Pts',(-0.184170554683796,-0.197991731059171,
-4.56769894905828));
#28319=CARTESIAN_POINT('Ctrl Pts',(0.0491753813860615,-0.276035885831286,
-4.55313512547041));
#28320=CARTESIAN_POINT('Ctrl Pts',(0.258642791859093,-0.108249409330772,
-4.53724954004591));
#28321=CARTESIAN_POINT('Ctrl Pts',(0.231132711334074,0.158718928148119,
-4.5213639546214));
#28322=CARTESIAN_POINT('Ctrl Pts',(-0.00814917085540682,0.280263482129757,
-4.50547836919689));
#28323=CARTESIAN_POINT('Ctrl Pts',(-0.204777283366198,0.165549369232331,
-4.49200405459293));
#28324=CARTESIAN_POINT('Ctrl Pts',(-0.236705400940218,0.0430794593642273,
-4.48382493513046));
#28325=CARTESIAN_POINT('Ctrl Pts',(-0.236798869759374,-5.74984565626727E-5,
-4.4809410108095));
#28326=CARTESIAN_POINT('Origin',(0.,0.,-6.1506589891905));
#28327=CARTESIAN_POINT('',(-0.236908709036994,-0.00016298456995,-4.7006589891905));
#28328=CARTESIAN_POINT('',(-0.237543953866199,-6.55533299058764E-5,-4.6809410108095));
#28329=CARTESIAN_POINT('',(-0.237175,1.98931295048561E-15,-6.1506589891905));
#28330=CARTESIAN_POINT('Ctrl Pts',(-0.236908709036994,-0.000162984569950002,
-4.7006589891905));
#28331=CARTESIAN_POINT('Ctrl Pts',(-0.237088327609357,-0.0285786996968505,
-4.69875704814015));
#28332=CARTESIAN_POINT('Ctrl Pts',(-0.21920122513728,-0.135888036726437,
-4.6915599119483));
#28333=CARTESIAN_POINT('Ctrl Pts',(-0.0595908711013016,-0.273976209565238,
-4.67906758061494));
#28334=CARTESIAN_POINT('Ctrl Pts',(0.197973181209263,-0.198546354406802,
-4.66318199519043));
#28335=CARTESIAN_POINT('Ctrl Pts',(0.274147342733956,0.0587985526884655,
-4.64729640976593));
#28336=CARTESIAN_POINT('Ctrl Pts',(0.0991382063290872,0.262270187730513,
-4.63141082434142));
#28337=CARTESIAN_POINT('Ctrl Pts',(-0.161018645402043,0.226228534144202,
-4.61586501748294));
#28338=CARTESIAN_POINT('Ctrl Pts',(-0.237163185334549,0.0734532857575236,
-4.60561440576597));
#28339=CARTESIAN_POINT('Ctrl Pts',(-0.237523476840667,-9.09874636312079E-5,
-4.6006589891905));
#28340=CARTESIAN_POINT('Ctrl Pts',(-0.237543953866199,-6.55533299058803E-5,
-4.6809410108095));
#28341=CARTESIAN_POINT('Ctrl Pts',(-0.237557049209306,-0.00363256502421958,
-4.68070061016182));
#28342=CARTESIAN_POINT('Ctrl Pts',(-0.235867300532786,-0.0857558329936854,
-4.67516501437264));
#28343=CARTESIAN_POINT('Ctrl Pts',(-0.141103532512842,-0.242288715200532,
-4.66433422344196));
#28344=CARTESIAN_POINT('Ctrl Pts',(0.127170996645068,-0.249883104697832,
-4.64844863801745));
#28345=CARTESIAN_POINT('Ctrl Pts',(0.278927050665701,-0.0285259322031912,
-4.63256305259295));
#28346=CARTESIAN_POINT('Ctrl Pts',(0.175120472675097,0.218967688144114,
-4.61667746716844));
#28347=CARTESIAN_POINT('Ctrl Pts',(-0.0891375524199996,0.265835522738591,
-4.60079188174394));
#28348=CARTESIAN_POINT('Ctrl Pts',(-0.226054472369514,0.118335830510633,
-4.58887972962428));
#28349=CARTESIAN_POINT('Ctrl Pts',(-0.237314661903335,0.0199169633854095,
-4.58226277264614));
#28350=CARTESIAN_POINT('Ctrl Pts',(-0.237136177256987,0.000217231692762269,
-4.5809410108095));
#28351=CARTESIAN_POINT('Origin',(0.,0.,-6.1506589891905));
#28352=CARTESIAN_POINT('',(-0.236931796274552,0.000174130487424274,-4.8006589891905));
#28353=CARTESIAN_POINT('',(-0.236941539607102,-0.000178305245891713,-4.7809410108095));
#28354=CARTESIAN_POINT('',(-0.237175,1.98931295048561E-15,-6.1506589891905));
#28355=CARTESIAN_POINT('Ctrl Pts',(-0.236931796274552,0.000174130487424283,
-4.8006589891905));
#28356=CARTESIAN_POINT('Ctrl Pts',(-0.236580090821685,-0.0515682065233269,
-4.79719488565583));
#28357=CARTESIAN_POINT('Ctrl Pts',(-0.194440311842266,-0.18292465151328,
-4.78843558697966));
#28358=CARTESIAN_POINT('Ctrl Pts',(0.0224884069277866,-0.279478634031651,
-4.77438109316199));
#28359=CARTESIAN_POINT('Ctrl Pts',(0.247075054914963,-0.13254415326643,
-4.75849550773747));
#28360=CARTESIAN_POINT('Ctrl Pts',(0.245282973454107,0.135831874977338,
-4.74260992231297));
#28361=CARTESIAN_POINT('Ctrl Pts',(0.0187541296969196,0.279754031151758,
-4.72672433688846));
#28362=CARTESIAN_POINT('Ctrl Pts',(-0.19577887178785,0.180812998027858,
-4.71274069251431));
#28363=CARTESIAN_POINT('Ctrl Pts',(-0.23658825144163,0.0505335086728689,
-4.70405224328166));
#28364=CARTESIAN_POINT('Ctrl Pts',(-0.236908709036994,-0.000162984569950002,
-4.7006589891905));
#28365=CARTESIAN_POINT('Ctrl Pts',(-0.236941539607102,-0.000178305245891745,
-4.7809410108095));
#28366=CARTESIAN_POINT('Ctrl Pts',(-0.237129442313695,-0.0270998926955989,
-4.7791384476775));
#28367=CARTESIAN_POINT('Ctrl Pts',(-0.220459184495624,-0.132880385692709,
-4.772040689404));
#28368=CARTESIAN_POINT('Ctrl Pts',(-0.0647123167632992,-0.272811921404205,
-4.759647735989));
#28369=CARTESIAN_POINT('Ctrl Pts',(0.194219427751849,-0.202219787075528,
-4.7437621505645));
#28370=CARTESIAN_POINT('Ctrl Pts',(0.275200600511704,0.0536531255298783,
-4.72787656513998));
#28371=CARTESIAN_POINT('Ctrl Pts',(0.104033444057923,0.260367184795962,
-4.71199097971549));
#28372=CARTESIAN_POINT('Ctrl Pts',(-0.158419955632031,0.229005698543907,
-4.69634579493865));
#28373=CARTESIAN_POINT('Ctrl Pts',(-0.23726860407462,0.0749363705253955,
-4.68599580530332));
#28374=CARTESIAN_POINT('Ctrl Pts',(-0.237543953866199,-6.55533299058803E-5,
-4.6809410108095));
#28375=CARTESIAN_POINT('Origin',(0.,0.,-6.1506589891905));
#28376=CARTESIAN_POINT('',(-0.237538693477751,7.2995197219953E-5,-4.9006589891905));
#28377=CARTESIAN_POINT('',(-0.236899879648722,0.000158196596847071,-4.88094101080949));
#28378=CARTESIAN_POINT('',(-0.237175,1.98931295048561E-15,-6.1506589891905));
#28379=CARTESIAN_POINT('Ctrl Pts',(-0.237538693477751,7.29951972199385E-5,
-4.9006589891905));
#28380=CARTESIAN_POINT('Ctrl Pts',(-0.237237326520422,-0.0745100491991757,
-4.89563272317151));
#28381=CARTESIAN_POINT('Ctrl Pts',(-0.159170881587928,-0.228210259049412,
-4.88531126201102));
#28382=CARTESIAN_POINT('Ctrl Pts',(0.102631828995819,-0.260922867919469,
-4.86969460570902));
#28383=CARTESIAN_POINT('Ctrl Pts',(0.274908115786522,-0.0551322337752745,
-4.85380902028452));
#28384=CARTESIAN_POINT('Ctrl Pts',(0.195304058006928,0.201172463951639,
-4.83792343486001));
#28385=CARTESIAN_POINT('Ctrl Pts',(-0.0632443473631996,0.273155977150327,
-4.82203784943551));
#28386=CARTESIAN_POINT('Ctrl Pts',(-0.220101702028949,0.13374379324399,
-4.80961636754567));
#28387=CARTESIAN_POINT('Ctrl Pts',(-0.237117704373537,0.0275246291287032,
-4.80249008079733));
#28388=CARTESIAN_POINT('Ctrl Pts',(-0.236931796274552,0.000174130487424283,
-4.8006589891905));
#28389=CARTESIAN_POINT('Ctrl Pts',(-0.236899879648722,0.000158196596847054,
-4.88094101080949));
#28390=CARTESIAN_POINT('Ctrl Pts',(-0.236592171127761,-0.050116767091128,
-4.87757628519318));
#28391=CARTESIAN_POINT('Ctrl Pts',(-0.196311764217322,-0.179961785169845,
-4.86891636443536));
#28392=CARTESIAN_POINT('Ctrl Pts',(0.0172494902941208,-0.279850823628805,
-4.85496124853605));
#28393=CARTESIAN_POINT('Ctrl Pts',(0.244548985077421,-0.137148905568842,
-4.83907566311153));
#28394=CARTESIAN_POINT('Ctrl Pts',(0.247784223156673,0.131213593639424,
-4.82319007768704));
#28395=CARTESIAN_POINT('Ctrl Pts',(0.0239909672635905,0.279353650219367,
-4.80730449226251));
#28396=CARTESIAN_POINT('Ctrl Pts',(-0.193895200773842,0.183773975398,-4.79322146997002));
#28397=CARTESIAN_POINT('Ctrl Pts',(-0.236577460815037,0.0519847487989422,
-4.78443364281901));
#28398=CARTESIAN_POINT('Ctrl Pts',(-0.236941539607102,-0.000178305245891745,
-4.7809410108095));
#28399=CARTESIAN_POINT('Origin',(0.,0.,-6.1506589891905));
#28400=CARTESIAN_POINT('',(-0.237148948645665,-0.00021749005109032,-5.0006589891905));
#28401=CARTESIAN_POINT('',(-0.237516529348539,9.80111424561253E-5,-4.9809410108095));
#28402=CARTESIAN_POINT('',(-0.237175,1.98931295048561E-15,-6.1506589891905));
#28403=CARTESIAN_POINT('Ctrl Pts',(-0.237148948645665,-0.000217490051090299,
-5.0006589891905));
#28404=CARTESIAN_POINT('Ctrl Pts',(-0.237324608020506,-0.0194893848684046,
-4.99936575582869));
#28405=CARTESIAN_POINT('Ctrl Pts',(-0.226361561945563,-0.117473530672288,
-4.99277732732538));
#28406=CARTESIAN_POINT('Ctrl Pts',(-0.0905657887914961,-0.265352356738962,
-4.98089370368057));
#28407=CARTESIAN_POINT('Ctrl Pts',(0.173940457270164,-0.219906236043896,
-4.96500811825607));
#28408=CARTESIAN_POINT('Ctrl Pts',(0.279076427243118,0.0270256005218002,
-4.94912253283156));
#28409=CARTESIAN_POINT('Ctrl Pts',(0.128512901206904,0.249195645125937,
-4.93323694740706));
#28410=CARTESIAN_POINT('Ctrl Pts',(-0.139798599439343,0.243044002026681,
-4.91735136198254));
#28411=CARTESIAN_POINT('Ctrl Pts',(-0.235654574442953,0.0866120031589777,
-4.90649204257703));
#28412=CARTESIAN_POINT('Ctrl Pts',(-0.237554818042404,0.00406354257534346,
-4.90092791831301));
#28413=CARTESIAN_POINT('Ctrl Pts',(-0.237538693477751,7.29951972199385E-5,
-4.9006589891905));
#28414=CARTESIAN_POINT('Ctrl Pts',(-0.237516529348539,9.80111424561452E-5,
-4.9809410108095));
#28415=CARTESIAN_POINT('Ctrl Pts',(-0.237134737314428,-0.0730285328966137,
-4.97601412270886));
#28416=CARTESIAN_POINT('Ctrl Pts',(-0.161755788795796,-0.225428088374244,
-4.96579203946672));
#28417=CARTESIAN_POINT('Ctrl Pts',(0.0977264198891994,-0.262799496302347,
-4.95027476108308));
#28418=CARTESIAN_POINT('Ctrl Pts',(0.273827179714107,-0.0602719175980483,
-4.93438917565858));
#28419=CARTESIAN_POINT('Ctrl Pts',(0.199037986065754,0.197478881159522,
-4.91850359023406));
#28420=CARTESIAN_POINT('Ctrl Pts',(-0.0581167094863374,0.274292683970259,
-4.90261800480957));
#28421=CARTESIAN_POINT('Ctrl Pts',(-0.218833502316203,0.136751428414759,
-4.89009714500137));
#28422=CARTESIAN_POINT('Ctrl Pts',(-0.237076423590217,0.0290028324889566,
-4.88287148033468));
#28423=CARTESIAN_POINT('Ctrl Pts',(-0.236899879648722,0.000158196596847054,
-4.88094101080949));
#28424=CARTESIAN_POINT('Origin',(0.,0.,-6.1506589891905));
#28425=CARTESIAN_POINT('',(-0.236795980310558,5.06907052245788E-5,-5.1006589891905));
#28426=CARTESIAN_POINT('',(-0.237193800648222,-0.000216474445068449,-5.0809410108095));
#28427=CARTESIAN_POINT('',(-0.237175,1.98931295048561E-15,-6.1506589891905));
#28428=CARTESIAN_POINT('Ctrl Pts',(-0.236795980310558,5.06907052245723E-5,
-5.1006589891905));
#28429=CARTESIAN_POINT('Ctrl Pts',(-0.23671444927506,-0.0426608529623053,
-5.09780359334437));
#28430=CARTESIAN_POINT('Ctrl Pts',(-0.205249568998764,-0.164690913697368,
-5.08965300235675));
#28431=CARTESIAN_POINT('Ctrl Pts',(-0.00965616049258788,-0.280215620354914,
-5.07620721622762));
#28432=CARTESIAN_POINT('Ctrl Pts',(0.230275874140234,-0.159959548371763,
-5.0603216308031));
#28433=CARTESIAN_POINT('Ctrl Pts',(0.25922117104535,0.106857006360016,-5.04443604537861));
#28434=CARTESIAN_POINT('Ctrl Pts',(0.0506590458941416,0.275767467978807,
-5.02855045995409));
#28435=CARTESIAN_POINT('Ctrl Pts',(-0.183561113561564,0.198828830534759,
-5.0139581078914));
#28436=CARTESIAN_POINT('Ctrl Pts',(-0.23660536376368,0.0594201505781383,
-5.0046609509702));
#28437=CARTESIAN_POINT('Ctrl Pts',(-0.237148948645665,-0.000217490051090299,
-5.0006589891905));
#28438=CARTESIAN_POINT('Ctrl Pts',(-0.237193800648222,-0.000216474445068456,
-5.0809410108095));
#28439=CARTESIAN_POINT('Ctrl Pts',(-0.237358018819269,-0.0179988291517084,
-5.07974715536605));
#28440=CARTESIAN_POINT('Ctrl Pts',(-0.22741001665069,-0.11447059654328,
-5.07325810478109));
#28441=CARTESIAN_POINT('Ctrl Pts',(-0.0955202636039318,-0.26360938458667,
-5.06147385905463));
#28442=CARTESIAN_POINT('Ctrl Pts',(0.169790825062137,-0.223125758544025,
-5.04558827363013));
#28443=CARTESIAN_POINT('Ctrl Pts',(0.279533674503372,0.0217934214792116,
-5.02970268820562));
#28444=CARTESIAN_POINT('Ctrl Pts',(0.133158082146451,0.246744713337908,
-5.01381710278111));
#28445=CARTESIAN_POINT('Ctrl Pts',(-0.135221560608942,0.245619946151793,
-4.99793151735661));
#28446=CARTESIAN_POINT('Ctrl Pts',(-0.234894750020545,0.0895960082762632,
-4.98697282003273));
#28447=CARTESIAN_POINT('Ctrl Pts',(-0.23754507001994,0.00556454914650678,
-4.98130931785036));
#28448=CARTESIAN_POINT('Ctrl Pts',(-0.237516529348539,9.80111424561452E-5,
-4.9809410108095));
#28449=CARTESIAN_POINT('Origin',(0.,0.,-6.1506589891905));
#28450=CARTESIAN_POINT('',(-0.237335164775886,0.000193322802161542,-5.2006589891905));
#28451=CARTESIAN_POINT('',(-0.236788752274853,2.66210406855288E-5,-5.1809410108095));
#28452=CARTESIAN_POINT('',(-0.237175,1.98931295048561E-15,-6.1506589891905));
#28453=CARTESIAN_POINT('Ctrl Pts',(-0.237335164775886,0.00019332280216155,
-5.2006589891905));
#28454=CARTESIAN_POINT('Ctrl Pts',(-0.236755294092649,-0.0655048792155798,
-5.19624143086006));
#28455=CARTESIAN_POINT('Ctrl Pts',(-0.174259926607873,-0.210921685958696,
-5.18652867738811));
#28456=CARTESIAN_POINT('Ctrl Pts',(0.0720846932421861,-0.270957251843399,
-5.17152072877465));
#28457=CARTESIAN_POINT('Ctrl Pts',(0.266788591915922,-0.0862431594381096,
-5.15563514335015));
#28458=CARTESIAN_POINT('Ctrl Pts',(0.217051535229177,0.177489905011538,
-5.13974955792564));
#28459=CARTESIAN_POINT('Ctrl Pts',(-0.0315556614918893,0.278600566320595,
-5.12386397250114));
#28460=CARTESIAN_POINT('Ctrl Pts',(-0.211760853398221,0.152156333831052,
-5.11083378292275));
#28461=CARTESIAN_POINT('Ctrl Pts',(-0.236865644684144,0.0365456636476937,
-5.10309878848588));
#28462=CARTESIAN_POINT('Ctrl Pts',(-0.236795980310558,5.06907052245723E-5,
-5.1006589891905));
#28463=CARTESIAN_POINT('Ctrl Pts',(-0.236788752274853,2.66210406855358E-5,
-5.1809410108095));
#28464=CARTESIAN_POINT('Ctrl Pts',(-0.236747495401724,-0.0412015421027071,
-5.17818499288173));
#28465=CARTESIAN_POINT('Ctrl Pts',(-0.206869023211992,-0.161698214308556,
-5.17013377981245));
#28466=CARTESIAN_POINT('Ctrl Pts',(-0.0149032407667099,-0.279985574299422,
-5.15678737160167));
#28467=CARTESIAN_POINT('Ctrl Pts',(0.22723922911572,-0.164244820776854,
-5.14090178617716));
#28468=CARTESIAN_POINT('Ctrl Pts',(0.261177240698333,0.101982730608336,
-5.12501620075266));
#28469=CARTESIAN_POINT('Ctrl Pts',(0.0558156114071165,0.274770169276757,
-5.10913061532815));
#28470=CARTESIAN_POINT('Ctrl Pts',(-0.181409236364921,0.201738255249697,
-5.0944388853471));
#28471=CARTESIAN_POINT('Ctrl Pts',(-0.236629649847762,0.0608725608171928,
-5.08504235050755));
#28472=CARTESIAN_POINT('Ctrl Pts',(-0.237193800648222,-0.000216474445068456,
-5.0809410108095));
#28473=CARTESIAN_POINT('Origin',(0.,0.,-6.1506589891905));
#28474=CARTESIAN_POINT('',(-0.237414200045941,-0.000164802835073178,-5.3006589891905));
#28475=CARTESIAN_POINT('',(-0.237291647891957,0.000203839981857537,-5.2809410108095));
#28476=CARTESIAN_POINT('',(-0.237175,1.98931295048561E-15,-6.1506589891905));
#28477=CARTESIAN_POINT('Ctrl Pts',(-0.237414200045941,-0.000164802835073157,
-5.3006589891905));
#28478=CARTESIAN_POINT('Ctrl Pts',(-0.237494743202661,-0.0103362946657776,
-5.29997446351724));
#28479=CARTESIAN_POINT('Ctrl Pts',(-0.232279536649386,-0.0991068806287269,
-5.29399474270247));
#28480=CARTESIAN_POINT('Ctrl Pts',(-0.120349718205416,-0.253238979334194,
-5.28271982674621));
#28481=CARTESIAN_POINT('Ctrl Pts',(0.147620323834129,-0.23837423375326,
-5.2668342413217));
#28482=CARTESIAN_POINT('Ctrl Pts',(0.280335508349595,-0.00510275266119098,
-5.25094865589719));
#28483=CARTESIAN_POINT('Ctrl Pts',(0.156197583103769,0.232844047291076,
-5.23506307047268));
#28484=CARTESIAN_POINT('Ctrl Pts',(-0.111053981914616,0.257451060256615,
-5.21917748504818));
#28485=CARTESIAN_POINT('Ctrl Pts',(-0.230530796392364,0.104926093377206,
-5.20770945795412));
#28486=CARTESIAN_POINT('Ctrl Pts',(-0.237450367749835,0.0132455919965611,
-5.20153662600156));
#28487=CARTESIAN_POINT('Ctrl Pts',(-0.237335164775886,0.00019332280216155,
-5.2006589891905));
#28488=CARTESIAN_POINT('Ctrl Pts',(-0.237291647891957,0.000203839981857532,
-5.2809410108095));
#28489=CARTESIAN_POINT('Ctrl Pts',(-0.236707472807153,-0.0640468622466563,
-5.27662283039741));
#28490=CARTESIAN_POINT('Ctrl Pts',(-0.176556678251362,-0.20804859565348,
-5.26700945484381));
#28491=CARTESIAN_POINT('Ctrl Pts',(0.0669966887508262,-0.272259934800463,
-5.25210088414871));
#28492=CARTESIAN_POINT('Ctrl Pts',(0.265126335755849,-0.0912252952300192,
-5.23621529872421));
#28493=CARTESIAN_POINT('Ctrl Pts',(0.220338044111505,0.173393121888511,
-5.2203297132997));
#28494=CARTESIAN_POINT('Ctrl Pts',(-0.0263316009223782,0.279142750566788,
-5.2044441278752));
#28495=CARTESIAN_POINT('Ctrl Pts',(-0.210265822348046,0.155157722278446,
-5.19131456037846));
#28496=CARTESIAN_POINT('Ctrl Pts',(-0.236826763098768,0.0380109938427312,
-5.18348018802323));
#28497=CARTESIAN_POINT('Ctrl Pts',(-0.236788752274853,2.66210406855358E-5,
-5.1809410108095));
#28498=CARTESIAN_POINT('Origin',(0.,0.,-6.1506589891905));
#28499=CARTESIAN_POINT('',(-0.236822660016195,-9.54250159434449E-5,-5.4006589891905));
#28500=CARTESIAN_POINT('',(-0.237450728442205,-0.000146260240270479,-5.3809410108095));
#28501=CARTESIAN_POINT('',(-0.237175,1.98931295048561E-15,-6.1506589891905));
#28502=CARTESIAN_POINT('Ctrl Pts',(-0.236822660016195,-9.54250159434407E-5,
-5.4006589891905));
#28503=CARTESIAN_POINT('Ctrl Pts',(-0.236944197811255,-0.0336923528614689,
-5.39841230103292));
#28504=CARTESIAN_POINT('Ctrl Pts',(-0.214557208673931,-0.146318914545383,
-5.39087041773384));
#28505=CARTESIAN_POINT('Ctrl Pts',(-0.0416737442683253,-0.27726762228038,
-5.37803333929325));
#28506=CARTESIAN_POINT('Ctrl Pts',(0.21044844318329,-0.185271390365794,
-5.36214775386874));
#28507=CARTESIAN_POINT('Ctrl Pts',(0.269750472409913,0.0764769112933738,
-5.34626216844423));
#28508=CARTESIAN_POINT('Ctrl Pts',(0.0818977687025324,0.268154415976868,
-5.33037658301972));
#28509=CARTESIAN_POINT('Ctrl Pts',(-0.169664305922363,0.216467104244653,
-5.31517552326848));
#28510=CARTESIAN_POINT('Ctrl Pts',(-0.236871696107715,0.0683459757405056,
-5.30526965865874));
#28511=CARTESIAN_POINT('Ctrl Pts',(-0.237414200045941,-0.000164802835073157,
-5.3006589891905));
#28512=CARTESIAN_POINT('Ctrl Pts',(-0.237450728442205,-0.000146260240270466,
-5.3809410108095));
#28513=CARTESIAN_POINT('Ctrl Pts',(-0.237513641523012,-0.0088375729951032,
-5.38035586305459));
#28514=CARTESIAN_POINT('Ctrl Pts',(-0.233134227691199,-0.0961153864525537,
-5.37447552015817));
#28515=CARTESIAN_POINT('Ctrl Pts',(-0.125072068190222,-0.250940244201183,
-5.36329998212027));
#28516=CARTESIAN_POINT('Ctrl Pts',(0.143129382745379,-0.241097507652099,
-5.34741439669575));
#28517=CARTESIAN_POINT('Ctrl Pts',(0.280190732047764,-0.0103528776514324,
-5.33152881127125));
#28518=CARTESIAN_POINT('Ctrl Pts',(0.160531620654842,0.229877417705736,
-5.31564322584674));
#28519=CARTESIAN_POINT('Ctrl Pts',(-0.10621212594168,0.259486054931813,
-5.29975764042223));
#28520=CARTESIAN_POINT('Ctrl Pts',(-0.229584869499672,0.107923695599517,
-5.28819023540982));
#28521=CARTESIAN_POINT('Ctrl Pts',(-0.237423821077868,0.0147409543359568,
-5.28191802553891));
#28522=CARTESIAN_POINT('Ctrl Pts',(-0.237291647891957,0.000203839981857532,
-5.2809410108095));
#28523=CARTESIAN_POINT('Origin',(0.,0.,-6.1506589891905));
#28524=CARTESIAN_POINT('',(-0.237064417961372,0.000211057165585043,-5.5006589891905));
#28525=CARTESIAN_POINT('',(-0.236842640230931,-0.000116843745555151,-5.4809410108095));
#28526=CARTESIAN_POINT('',(-0.237175,1.98931295048561E-15,-6.1506589891905));
#28527=CARTESIAN_POINT('Ctrl Pts',(-0.237064417961372,0.000211057165585036,
-5.5006589891905));
#28528=CARTESIAN_POINT('Ctrl Pts',(-0.236576849557631,-0.0566003236648596,
-5.4968501385486));
#28529=CARTESIAN_POINT('Ctrl Pts',(-0.187614909420263,-0.193147175570037,
-5.48774609276519));
#28530=CARTESIAN_POINT('Ctrl Pts',(0.040589605444914,-0.277428403839015,
-5.47334685184029));
#28531=CARTESIAN_POINT('Ctrl Pts',(0.255160656210713,-0.116219941698528,
-5.45746126641578));
#28532=CARTESIAN_POINT('Ctrl Pts',(0.235944669357195,0.151473259449223,
-5.44157568099128));
#28533=CARTESIAN_POINT('Ctrl Pts',(0.000547998106158669,0.280381409912451,
-5.42569009556676));
#28534=CARTESIAN_POINT('Ctrl Pts',(-0.201987756818871,0.170495515579157,
-5.41205119829984));
#28535=CARTESIAN_POINT('Ctrl Pts',(-0.236657746689972,0.0454918848337113,
-5.40370749617442));
#28536=CARTESIAN_POINT('Ctrl Pts',(-0.236822660016195,-9.54250159434407E-5,
-5.4006589891905));
#28537=CARTESIAN_POINT('Ctrl Pts',(-0.236842640230931,-0.000116843745555185,
-5.4809410108095));
#28538=CARTESIAN_POINT('Ctrl Pts',(-0.236985574897071,-0.0322208987592947,
-5.47879370057027));
#28539=CARTESIAN_POINT('Ctrl Pts',(-0.21594113561778,-0.143312950842703,
-5.47135119518954));
#28540=CARTESIAN_POINT('Ctrl Pts',(-0.0468599862874815,-0.276438365800292,
-5.45861349466731));
#28541=CARTESIAN_POINT('Ctrl Pts',(0.206941156468481,-0.189180829262909,
-5.4427279092428));
#28542=CARTESIAN_POINT('Ctrl Pts',(0.271135638657325,0.0714107404456813,
-5.42684232381829));
#28543=CARTESIAN_POINT('Ctrl Pts',(0.0869062505835863,0.266573314513364,
-5.41095673839378));
#28544=CARTESIAN_POINT('Ctrl Pts',(-0.167230487480177,0.219300088354176,
-5.39565630072419));
#28545=CARTESIAN_POINT('Ctrl Pts',(-0.236944320292551,0.0698129843838412,
-5.38565105819609));
#28546=CARTESIAN_POINT('Ctrl Pts',(-0.237450728442205,-0.000146260240270466,
-5.3809410108095));
#28547=CARTESIAN_POINT('Origin',(0.,0.,-6.1506589891905));
#28548=CARTESIAN_POINT('',(-0.237563686191593,-2.10269292758361E-5,-5.6006589891905));
#28549=CARTESIAN_POINT('',(-0.237023234876043,0.000203592057815866,-5.5809410108095));
#28550=CARTESIAN_POINT('',(-0.237175,1.98931295048561E-15,-6.1506589891905));
#28551=CARTESIAN_POINT('Ctrl Pts',(-0.237563686191593,-2.10269292758463E-5,
-5.6006589891905));
#28552=CARTESIAN_POINT('Ctrl Pts',(-0.237565111147283,-0.00114574716038694,
-5.60058317120578));
#28553=CARTESIAN_POINT('Ctrl Pts',(-0.237048263617325,-0.080820577600737,
-5.59521215807956));
#28554=CARTESIAN_POINT('Ctrl Pts',(-0.14855098481485,-0.237795374612464,
-5.58454594981183));
#28555=CARTESIAN_POINT('Ctrl Pts',(0.119358904639683,-0.253707483593214,
-5.56866036438733));
#28556=CARTESIAN_POINT('Ctrl Pts',(0.277908028472834,-0.0371640019089366,
-5.55277477896282));
#28557=CARTESIAN_POINT('Ctrl Pts',(0.181828183730025,0.21343042641883,-5.53688919353832));
#28558=CARTESIAN_POINT('Ctrl Pts',(-0.0808489454790468,0.268472500164499,
-5.52100360811381));
#28559=CARTESIAN_POINT('Ctrl Pts',(-0.224229150548578,0.123312428819558,
-5.5089268733312));
#28560=CARTESIAN_POINT('Ctrl Pts',(-0.237254683919062,0.0223808116009525,
-5.5021453336901));
#28561=CARTESIAN_POINT('Ctrl Pts',(-0.237064417961372,0.000211057165585036,
-5.5006589891905));
#28562=CARTESIAN_POINT('Ctrl Pts',(-0.237023234876043,0.000203592057815862,
-5.5809410108095));
#28563=CARTESIAN_POINT('Ctrl Pts',(-0.236571091847558,-0.0551498509335718,
-5.57723153808595));
#28564=CARTESIAN_POINT('Ctrl Pts',(-0.189636057293001,-0.190210103257596,
-5.56822687022089));
#28565=CARTESIAN_POINT('Ctrl Pts',(0.0353859155308252,-0.278140010402117,
-5.55392700721436));
#28566=CARTESIAN_POINT('Ctrl Pts',(0.252938939516514,-0.120979011722138,
-5.53804142178983));
#28567=CARTESIAN_POINT('Ctrl Pts',(0.238740539723166,0.147027150870172,
-5.52215583636534));
#28568=CARTESIAN_POINT('Ctrl Pts',(0.0057997821945244,0.280321941574533,
-5.50627025094082));
#28569=CARTESIAN_POINT('Ctrl Pts',(-0.200249211686888,0.173476183501598,
-5.49253197575555));
#28570=CARTESIAN_POINT('Ctrl Pts',(-0.23663310279692,0.0469466258142949,
-5.48408889571177));
#28571=CARTESIAN_POINT('Ctrl Pts',(-0.236842640230931,-0.000116843745555185,
-5.4809410108095));
#28572=CARTESIAN_POINT('Origin',(0.,0.,-6.1506589891905));
#28573=CARTESIAN_POINT('',(-0.237002443247224,-0.000198590235900253,-5.7006589891905));
#28574=CARTESIAN_POINT('',(-0.237565764759064,6.5451087111932E-6,-5.6809410108095));
#28575=CARTESIAN_POINT('',(-0.237175,1.98931295048561E-15,-6.1506589891905));
#28576=CARTESIAN_POINT('Ctrl Pts',(-0.237002443247224,-0.00019859023590026,
-5.7006589891905));
#28577=CARTESIAN_POINT('Ctrl Pts',(-0.237195969987065,-0.0246462657790171,
-5.69902100872146));
#28578=CARTESIAN_POINT('Ctrl Pts',(-0.222465081710047,-0.127899829220746,
-5.69208783311092));
#28579=CARTESIAN_POINT('Ctrl Pts',(-0.0731432950877003,-0.270673402752768,
-5.67985946235888));
#28580=CARTESIAN_POINT('Ctrl Pts',(0.187853502754299,-0.208146817550068,
-5.66397387693437));
#28581=CARTESIAN_POINT('Ctrl Pts',(0.276732411920541,0.0450911054647064,
-5.64808829150987));
#28582=CARTESIAN_POINT('Ctrl Pts',(0.112059492160603,0.257014990163246,
-5.63220270608536));
#28583=CARTESIAN_POINT('Ctrl Pts',(-0.154010242816776,0.23356529091088,
-5.61639293864557));
#28584=CARTESIAN_POINT('Ctrl Pts',(-0.237465590980955,0.0774057090053768,
-5.60587836634729));
#28585=CARTESIAN_POINT('Ctrl Pts',(-0.237563686191593,-2.10269292758463E-5,
-5.6006589891905));
#28586=CARTESIAN_POINT('Ctrl Pts',(-0.237565764759064,6.54510871119022E-6,
-5.6809410108095));
#28587=CARTESIAN_POINT('Ctrl Pts',(-0.2375341250678,-0.0781935536318626,
-5.67566937560163));
#28588=CARTESIAN_POINT('Ctrl Pts',(-0.152582282569065,-0.235002143286345,
-5.66510254525225));
#28589=CARTESIAN_POINT('Ctrl Pts',(0.114585712811833,-0.255898696670898,
-5.6492405197614));
#28590=CARTESIAN_POINT('Ctrl Pts',(0.277163132557144,-0.0423630307669099,
-5.63335493433687));
#28591=CARTESIAN_POINT('Ctrl Pts',(0.18579408296189,0.209987111717646,-5.61746934891238));
#28592=CARTESIAN_POINT('Ctrl Pts',(-0.0758059453271951,0.269939784166574,
-5.60158376348786));
#28593=CARTESIAN_POINT('Ctrl Pts',(-0.223082036136281,0.126318675930788,
-5.58940765078691));
#28594=CARTESIAN_POINT('Ctrl Pts',(-0.237216516614399,0.0238660373711741,
-5.58252673322745));
#28595=CARTESIAN_POINT('Ctrl Pts',(-0.237023234876043,0.000203592057815862,
-5.5809410108095));
#28596=CARTESIAN_POINT('Origin',(0.,0.,-6.1506589891905));
#28597=CARTESIAN_POINT('',(-0.236854733944756,0.000127784916100184,-5.8006589891905));
#28598=CARTESIAN_POINT('',(-0.237042509219701,-0.000207466451680183,-5.7809410108095));
#28599=CARTESIAN_POINT('',(-0.237175,1.98931295048561E-15,-6.1506589891905));
#28600=CARTESIAN_POINT('Ctrl Pts',(-0.236854733944756,0.000127784916100174,
-5.8006589891905));
#28601=CARTESIAN_POINT('Ctrl Pts',(-0.236621530291177,-0.0477109510420727,
-5.79745884623714));
#28602=CARTESIAN_POINT('Ctrl Pts',(-0.199318547468919,-0.175041983926161,
-5.78896350814228));
#28603=CARTESIAN_POINT('Ctrl Pts',(0.00856079809868226,-0.280250974663184,
-5.77517297490592));
#28604=CARTESIAN_POINT('Ctrl Pts',(0.240177193574594,-0.144668499352843,
-5.75928738948141));
#28605=CARTESIAN_POINT('Ctrl Pts',(0.251735020445761,0.123464726945526,
-5.74340180405691));
#28606=CARTESIAN_POINT('Ctrl Pts',(0.0326444435734673,0.278475054243476,
-5.72751621863239));
#28607=CARTESIAN_POINT('Ctrl Pts',(-0.190681354952407,0.188662352749473,
-5.71326861367693));
#28608=CARTESIAN_POINT('Ctrl Pts',(-0.236570344790718,0.0543871630095648,
-5.70431620386297));
#28609=CARTESIAN_POINT('Ctrl Pts',(-0.237002443247224,-0.00019859023590026,
-5.7006589891905));
#28610=CARTESIAN_POINT('Ctrl Pts',(-0.237042509219701,-0.000207466451680186,
-5.7809410108095));
#28611=CARTESIAN_POINT('Ctrl Pts',(-0.23723477238687,-0.0231620637174002,
-5.77940240825881));
#28612=CARTESIAN_POINT('Ctrl Pts',(-0.223630207594125,-0.12489320512256,
-5.77256861056662));
#28613=CARTESIAN_POINT('Ctrl Pts',(-0.0782004847763744,-0.269255812835206,
-5.76043961773294));
#28614=CARTESIAN_POINT('Ctrl Pts',(0.183921690703183,-0.211629026318924,
-5.74455403230843));
#28615=CARTESIAN_POINT('Ctrl Pts',(0.277528462365728,0.0398996699056295,
-5.72866844688392));
#28616=CARTESIAN_POINT('Ctrl Pts',(0.116854024514864,0.254870874359421,
-5.71278286145941));
#28617=CARTESIAN_POINT('Ctrl Pts',(-0.150886114490242,0.236320565513686,
-5.69689727603491));
#28618=CARTESIAN_POINT('Ctrl Pts',(-0.237406868651535,0.0792549843919946,
-5.68628332581827));
#28619=CARTESIAN_POINT('Ctrl Pts',(-0.237565906162821,0.000356036123144353,
-5.68096457074313));
#28620=CARTESIAN_POINT('Ctrl Pts',(-0.237565764759064,6.54510871119022E-6,
-5.6809410108095));
#28621=CARTESIAN_POINT('Origin',(0.,0.,-6.1506589891905));
#28622=CARTESIAN_POINT('',(-0.237465179907044,0.000150546841787672,-5.9006589891905));
#28623=CARTESIAN_POINT('',(-0.23683200269258,0.000108453577955928,-5.8809410108095));
#28624=CARTESIAN_POINT('',(-0.237175,1.98931295048561E-15,-6.1506589891905));
#28625=CARTESIAN_POINT('Ctrl Pts',(-0.237465179907043,0.000150546841787677,
-5.9006589891905));
#28626=CARTESIAN_POINT('Ctrl Pts',(-0.236981875220679,-0.0705666565561128,
-5.89589668375282));
#28627=CARTESIAN_POINT('Ctrl Pts',(-0.165937056871875,-0.220807750888229,
-5.88583918317364));
#28628=CARTESIAN_POINT('Ctrl Pts',(0.0895307381976737,-0.265691300918094,
-5.87048648745296));
#28629=CARTESIAN_POINT('Ctrl Pts',(0.271824417221856,-0.0687432732808278,
-5.85460090202845));
#28630=CARTESIAN_POINT('Ctrl Pts',(0.205068419513521,0.191213573408882,
-5.83871531660395));
#28631=CARTESIAN_POINT('Ctrl Pts',(-0.0495811020651061,0.275961577584089,
-5.82282973117944));
#28632=CARTESIAN_POINT('Ctrl Pts',(-0.216653989164255,0.141732282719992,
-5.81014428870829));
#28633=CARTESIAN_POINT('Ctrl Pts',(-0.237007406444652,0.0314465884532806,
-5.80275404137865));
#28634=CARTESIAN_POINT('Ctrl Pts',(-0.236854733944756,0.000127784916100174,
-5.8006589891905));
#28635=CARTESIAN_POINT('Ctrl Pts',(-0.23683200269258,0.000108453577955931,
-5.8809410108095));
#28636=CARTESIAN_POINT('Ctrl Pts',(-0.23664399711632,-0.0462561242652418,
-5.87784024577449));
#28637=CARTESIAN_POINT('Ctrl Pts',(-0.201079717648982,-0.172066122555996,
-5.86944428559799));
#28638=CARTESIAN_POINT('Ctrl Pts',(0.00331049150882867,-0.28036067894795,
-5.85575313027998));
#28639=CARTESIAN_POINT('Ctrl Pts',(0.237424903254865,-0.149142678857182,
-5.83986754485547));
#28640=CARTESIAN_POINT('Ctrl Pts',(0.254003655790197,0.118728154629452,
-5.82398195943097));
#28641=CARTESIAN_POINT('Ctrl Pts',(0.0378547991123291,0.277814511990848,
-5.80809637400645));
#28642=CARTESIAN_POINT('Ctrl Pts',(-0.188683159783408,0.191603849320789,
-5.79374939113264));
#28643=CARTESIAN_POINT('Ctrl Pts',(-0.236573086892959,0.0558375920822262,
-5.78469760340032));
#28644=CARTESIAN_POINT('Ctrl Pts',(-0.237042509219701,-0.000207466451680186,
-5.7809410108095));
#28645=CARTESIAN_POINT('Ctrl Pts',(-0.103908919352507,0.213201587949045,
-5.99872339910054));
#28646=CARTESIAN_POINT('Ctrl Pts',(-0.174842563682769,0.178630371106822,
-5.99342820395904));
#28647=CARTESIAN_POINT('Ctrl Pts',(-0.278254691691039,0.0337029669877049,
-5.98283781367603));
#28648=CARTESIAN_POINT('Ctrl Pts',(-0.178944516740793,-0.216088258093402,
-5.96695222825153));
#28649=CARTESIAN_POINT('Ctrl Pts',(0.0845713142691825,-0.267244828007485,
-5.95106664282702));
#28650=CARTESIAN_POINT('Ctrl Pts',(0.270472008799548,-0.0738624404218237,
-5.93518105740252));
#28651=CARTESIAN_POINT('Ctrl Pts',(0.208622919271946,0.187359333710957,
-5.91929547197799));
#28652=CARTESIAN_POINT('Ctrl Pts',(-0.0444078770673998,0.276831260195588,
-5.90340988655351));
#28653=CARTESIAN_POINT('Ctrl Pts',(-0.256732964979994,0.112704617543663,
-5.88752430112898));
#28654=CARTESIAN_POINT('Ctrl Pts',(-0.233839555517391,-0.154708578258498,
-5.87163871570449));
#28655=CARTESIAN_POINT('Ctrl Pts',(0.00331049150882867,-0.28036067894795,
-5.85575313027998));
#28656=CARTESIAN_POINT('Ctrl Pts',(0.237424903254865,-0.149142678857182,
-5.83986754485547));
#28657=CARTESIAN_POINT('Ctrl Pts',(0.254003655790197,0.118728154629452,
-5.82398195943097));
#28658=CARTESIAN_POINT('Ctrl Pts',(0.0378547991123291,0.277814511990848,
-5.80809637400645));
#28659=CARTESIAN_POINT('Ctrl Pts',(-0.212977597467589,0.182358424924104,
-5.79221078858196));
#28660=CARTESIAN_POINT('Ctrl Pts',(-0.268672712500568,-0.0801812071883245,
-5.77632520315744));
#28661=CARTESIAN_POINT('Ctrl Pts',(-0.0782004847763744,-0.269255812835206,
-5.76043961773294));
#28662=CARTESIAN_POINT('Ctrl Pts',(0.183921690703183,-0.211629026318924,
-5.74455403230843));
#28663=CARTESIAN_POINT('Ctrl Pts',(0.277528462365728,0.0398996699056295,
-5.72866844688392));
#28664=CARTESIAN_POINT('Ctrl Pts',(0.116854024514864,0.254870874359421,
-5.71278286145941));
#28665=CARTESIAN_POINT('Ctrl Pts',(-0.150886114490242,0.236320565513686,
-5.69689727603491));
#28666=CARTESIAN_POINT('Ctrl Pts',(-0.280379168741369,0.00124515482944624,
-5.6810116906104));
#28667=CARTESIAN_POINT('Ctrl Pts',(-0.15297910832401,-0.23497110554711,
-5.66512610518589));
#28668=CARTESIAN_POINT('Ctrl Pts',(0.114585712811833,-0.255898696670898,
-5.6492405197614));
#28669=CARTESIAN_POINT('Ctrl Pts',(0.277163132557144,-0.0423630307669099,
-5.63335493433687));
#28670=CARTESIAN_POINT('Ctrl Pts',(0.18579408296189,0.209987111717646,-5.61746934891238));
#28671=CARTESIAN_POINT('Ctrl Pts',(-0.0758059453271951,0.269939784166574,
-5.60158376348786));
#28672=CARTESIAN_POINT('Ctrl Pts',(-0.267949938980526,0.0825642695277862,
-5.58569817806337));
#28673=CARTESIAN_POINT('Ctrl Pts',(-0.214588910804631,-0.180459490618597,
-5.56981259263885));
#28674=CARTESIAN_POINT('Ctrl Pts',(0.0353859155308252,-0.278140010402117,
-5.55392700721436));
#28675=CARTESIAN_POINT('Ctrl Pts',(0.252938939516514,-0.120979011722138,
-5.53804142178983));
#28676=CARTESIAN_POINT('Ctrl Pts',(0.238740539723166,0.147027150870172,
-5.52215583636534));
#28677=CARTESIAN_POINT('Ctrl Pts',(0.0057997821945244,0.280321941574533,
-5.50627025094082));
#28678=CARTESIAN_POINT('Ctrl Pts',(-0.232454936814486,0.15677605286409,
-5.49038466551632));
#28679=CARTESIAN_POINT('Ctrl Pts',(-0.257726385342159,-0.110413489662689,
-5.47449908009181));
#28680=CARTESIAN_POINT('Ctrl Pts',(-0.0468599862874815,-0.276438365800292,
-5.45861349466731));
#28681=CARTESIAN_POINT('Ctrl Pts',(0.206941156468481,-0.189180829262909,
-5.4427279092428));
#28682=CARTESIAN_POINT('Ctrl Pts',(0.271135638657325,0.0714107404456813,
-5.42684232381829));
#28683=CARTESIAN_POINT('Ctrl Pts',(0.0869062505835863,0.266573314513364,
-5.41095673839378));
#28684=CARTESIAN_POINT('Ctrl Pts',(-0.176949656626137,0.217492177838692,
-5.39507115296928));
#28685=CARTESIAN_POINT('Ctrl Pts',(-0.278678154992094,-0.0308628309026957,
-5.37918556754476));
#28686=CARTESIAN_POINT('Ctrl Pts',(-0.125072068190222,-0.250940244201183,
-5.36329998212027));
#28687=CARTESIAN_POINT('Ctrl Pts',(0.143129382745379,-0.241097507652099,
-5.34741439669575));
#28688=CARTESIAN_POINT('Ctrl Pts',(0.280190732047764,-0.0103528776514324,
-5.33152881127125));
#28689=CARTESIAN_POINT('Ctrl Pts',(0.160531620654842,0.229877417705736,
-5.31564322584674));
#28690=CARTESIAN_POINT('Ctrl Pts',(-0.10621212594168,0.259486054931813,
-5.29975764042223));
#28691=CARTESIAN_POINT('Ctrl Pts',(-0.27564064121739,0.0513445743033626,
-5.28387205499773));
#28692=CARTESIAN_POINT('Ctrl Pts',(-0.192517646732188,-0.203840585011494,
-5.26798646957322));
#28693=CARTESIAN_POINT('Ctrl Pts',(0.0669966887508262,-0.272259934800463,
-5.25210088414871));
#28694=CARTESIAN_POINT('Ctrl Pts',(0.265126335755849,-0.0912252952300192,
-5.23621529872421));
#28695=CARTESIAN_POINT('Ctrl Pts',(0.220338044111505,0.173393121888511,
-5.2203297132997));
#28696=CARTESIAN_POINT('Ctrl Pts',(-0.0263316009223782,0.279142750566788,
-5.2044441278752));
#28697=CARTESIAN_POINT('Ctrl Pts',(-0.248875320483161,0.129132115507845,
-5.18855854245069));
#28698=CARTESIAN_POINT('Ctrl Pts',(-0.24339084488138,-0.139193839766909,
-5.17267295702618));
#28699=CARTESIAN_POINT('Ctrl Pts',(-0.0149032407667099,-0.279985574299422,
-5.15678737160167));
#28700=CARTESIAN_POINT('Ctrl Pts',(0.22723922911572,-0.164244820776854,
-5.14090178617716));
#28701=CARTESIAN_POINT('Ctrl Pts',(0.261177240698333,0.101982730608336,
-5.12501620075266));
#28702=CARTESIAN_POINT('Ctrl Pts',(0.0558156114071165,0.274770169276757,
-5.10913061532815));
#28703=CARTESIAN_POINT('Ctrl Pts',(-0.200686215740403,0.195803654748638,
-5.09324502990364));
#28704=CARTESIAN_POINT('Ctrl Pts',(-0.273312375825205,-0.0625649552218312,
-5.07735944447914));
#28705=CARTESIAN_POINT('Ctrl Pts',(-0.0955202636039318,-0.26360938458667,
-5.06147385905463));
#28706=CARTESIAN_POINT('Ctrl Pts',(0.169790825062137,-0.223125758544025,
-5.04558827363013));
#28707=CARTESIAN_POINT('Ctrl Pts',(0.279533674503372,0.0217934214792116,
-5.02970268820562));
#28708=CARTESIAN_POINT('Ctrl Pts',(0.133158082146451,0.246744713337908,
-5.01381710278111));
#28709=CARTESIAN_POINT('Ctrl Pts',(-0.135221560608942,0.245619946151793,
-4.99793151735661));
#28710=CARTESIAN_POINT('Ctrl Pts',(-0.279706522474076,0.0194496706035552,
-4.9820459319321));
#28711=CARTESIAN_POINT('Ctrl Pts',(-0.167914673239027,-0.224541067317669,
-4.96616034650759));
#28712=CARTESIAN_POINT('Ctrl Pts',(0.0977264198891994,-0.262799496302347,
-4.95027476108308));
#28713=CARTESIAN_POINT('Ctrl Pts',(0.273827179714107,-0.0602719175980483,
-4.93438917565858));
#28714=CARTESIAN_POINT('Ctrl Pts',(0.199037986065754,0.197478881159522,
-4.91850359023406));
#28715=CARTESIAN_POINT('Ctrl Pts',(-0.0581167094863374,0.274292683970259,
-4.90261800480957));
#28716=CARTESIAN_POINT('Ctrl Pts',(-0.262022861361101,0.0997900221729051,
-4.88673241938505));
#28717=CARTESIAN_POINT('Ctrl Pts',(-0.225854585399838,-0.166143716868844,
-4.87084683396055));
#28718=CARTESIAN_POINT('Ctrl Pts',(0.0172494902941208,-0.279850823628805,
-4.85496124853605));
#28719=CARTESIAN_POINT('Ctrl Pts',(0.244548985077421,-0.137148905568842,
-4.83907566311153));
#28720=CARTESIAN_POINT('Ctrl Pts',(0.247784223156673,0.131213593639424,
-4.82319007768704));
#28721=CARTESIAN_POINT('Ctrl Pts',(0.0239909672635905,0.279353650219367,
-4.80730449226251));
#28722=CARTESIAN_POINT('Ctrl Pts',(-0.221783644413183,0.171540209490179,
-4.79141890683803));
#28723=CARTESIAN_POINT('Ctrl Pts',(-0.264352393596509,-0.093444317114117,
-4.77553332141351));
#28724=CARTESIAN_POINT('Ctrl Pts',(-0.0647123167632992,-0.272811921404205,
-4.759647735989));
#28725=CARTESIAN_POINT('Ctrl Pts',(0.194219427751849,-0.202219787075528,
-4.7437621505645));
#28726=CARTESIAN_POINT('Ctrl Pts',(0.275200600511704,0.0536531255298783,
-4.72787656513998));
#28727=CARTESIAN_POINT('Ctrl Pts',(0.104033444057923,0.260367184795962,
-4.71199097971549));
#28728=CARTESIAN_POINT('Ctrl Pts',(-0.162452759857131,0.228523804484191,
-4.69610539429097));
#28729=CARTESIAN_POINT('Ctrl Pts',(-0.280094114240769,-0.0127010066060424,
-4.68021980886647));
#28730=CARTESIAN_POINT('Ctrl Pts',(-0.141103532512842,-0.242288715200532,
-4.66433422344196));
#28731=CARTESIAN_POINT('Ctrl Pts',(0.127170996645068,-0.249883104697832,
-4.64844863801745));
#28732=CARTESIAN_POINT('Ctrl Pts',(0.278927050665701,-0.0285259322031912,
-4.63256305259295));
#28733=CARTESIAN_POINT('Ctrl Pts',(0.175120472675097,0.218967688144114,
-4.61667746716844));
#28734=CARTESIAN_POINT('Ctrl Pts',(-0.0891375524199996,0.265835522738591,
-4.60079188174394));
#28735=CARTESIAN_POINT('Ctrl Pts',(-0.271724662295054,0.0691356369882154,
-4.58490629631942));
#28736=CARTESIAN_POINT('Ctrl Pts',(-0.205348218033809,-0.190908715755637,
-4.56902071089492));
#28737=CARTESIAN_POINT('Ctrl Pts',(0.0491753813860615,-0.276035885831286,
-4.55313512547041));
#28738=CARTESIAN_POINT('Ctrl Pts',(0.258642791859093,-0.108249409330772,
-4.53724954004591));
#28739=CARTESIAN_POINT('Ctrl Pts',(0.231132711334074,0.158718928148119,
-4.5213639546214));
#28740=CARTESIAN_POINT('Ctrl Pts',(-0.00814917085540682,0.280263482129757,
-4.50547836919689));
#28741=CARTESIAN_POINT('Ctrl Pts',(-0.239964500239963,0.145020919269299,
-4.48959278377239));
#28742=CARTESIAN_POINT('Ctrl Pts',(-0.251916036836325,-0.123094836552177,
-4.47370719834787));
#28743=CARTESIAN_POINT('Ctrl Pts',(-0.0330533685498055,-0.278426836401662,
-4.45782161292337));
#28744=CARTESIAN_POINT('Ctrl Pts',(0.216093941700501,-0.178654517887089,
-4.44193602749886));
#28745=CARTESIAN_POINT('Ctrl Pts',(0.26724849229964,0.0848072624525569,
-4.42605044207435));
#28746=CARTESIAN_POINT('Ctrl Pts',(0.0735407108656338,0.270565689337182,
-4.41016485664985));
#28747=CARTESIAN_POINT('Ctrl Pts',(-0.187547618937357,0.208422453281923,
-4.39427927122535));
#28748=CARTESIAN_POINT('Ctrl Pts',(-0.276798319479655,-0.0446846588256681,
-4.37839368580083));
#28749=CARTESIAN_POINT('Ctrl Pts',(-0.112436805309618,-0.256850137654031,
-4.36250810037634));
#28750=CARTESIAN_POINT('Ctrl Pts',(0.154943207178462,-0.23368061740414,
-4.34662251495182));
#28751=CARTESIAN_POINT('Ctrl Pts',(0.280358882596026,0.00359518436732559,
-4.33073692952732));
#28752=CARTESIAN_POINT('Ctrl Pts',(0.14890003195752,0.237576953604884,-4.3148513441028));
#28753=CARTESIAN_POINT('Ctrl Pts',(-0.11898618914506,0.253882483038636,
-4.29896575867831));
#28754=CARTESIAN_POINT('Ctrl Pts',(-0.27785313944431,0.0375720814178366,
-4.28308017325379));
#28755=CARTESIAN_POINT('Ctrl Pts',(-0.182141412417354,-0.21316316352442,
-4.26719458782929));
#28756=CARTESIAN_POINT('Ctrl Pts',(0.0804545900663122,-0.268590929367298,
-4.25130900240478));
#28757=CARTESIAN_POINT('Ctrl Pts',(0.269335308407912,-0.0779263758039853,
-4.23542341698027));
#28758=CARTESIAN_POINT('Ctrl Pts',(0.211441681464576,0.184137024361096,
-4.21953783155577));
#28759=CARTESIAN_POINT('Ctrl Pts',(-0.0401821430447466,0.277487700234545,
-4.20365224613126));
#28760=CARTESIAN_POINT('Ctrl Pts',(-0.254989695299907,0.11659452685267,
-4.18776666070675));
#28761=CARTESIAN_POINT('Ctrl Pts',(-0.236166850248402,-0.151126593440284,
-4.17188107528225));
#28762=CARTESIAN_POINT('Ctrl Pts',(-0.000959750965527487,-0.280380290461363,
-4.15599548985773));
#28763=CARTESIAN_POINT('Ctrl Pts',(0.235126705419149,-0.152739846798193,
-4.14010990443324));
#28764=CARTESIAN_POINT('Ctrl Pts',(0.255781924318054,0.114846138782203,
-4.12422431900872));
#28765=CARTESIAN_POINT('Ctrl Pts',(0.0420808782244523,0.277206111204153,
-4.10833873358422));
#28766=CARTESIAN_POINT('Ctrl Pts',(-0.210176127110702,0.185580236001482,
-4.09245314815971));
#28767=CARTESIAN_POINT('Ctrl Pts',(-0.269862479642514,-0.076080684023625,
-4.07656756273521));
#28768=CARTESIAN_POINT('Ctrl Pts',(-0.0822914743374018,-0.268033844229383,
-4.0606819773107));
#28769=CARTESIAN_POINT('Ctrl Pts',(0.180677832160775,-0.214405105746405,
-4.04479639188619));
#28770=CARTESIAN_POINT('Ctrl Pts',(0.278103846141642,0.0356690223564828,
-4.02891080646169));
#28771=CARTESIAN_POINT('Ctrl Pts',(0.1207214766735,0.253061955797574,-4.01302522103717));
#28772=CARTESIAN_POINT('Ctrl Pts',(-0.14727009426389,0.238590753715125,
-3.99713963561268));
#28773=CARTESIAN_POINT('Ctrl Pts',(-0.280327699987403,0.00551443296643659,
-3.98125405018816));
#28774=CARTESIAN_POINT('Ctrl Pts',(-0.156539350554289,-0.232614402289902,
-3.96536846476366));
#28775=CARTESIAN_POINT('Ctrl Pts',(0.110675778439994,-0.257613859497429,
-3.94948287933915));
#28776=CARTESIAN_POINT('Ctrl Pts',(0.276485921807596,-0.0465785687612247,
-3.93359729391465));
#28777=CARTESIAN_POINT('Ctrl Pts',(0.188970082294562,0.207133620332956,
-3.91771170849014));
#28778=CARTESIAN_POINT('Ctrl Pts',(-0.0716867010729343,0.271062808441053,
-3.90182612306563));
#28779=CARTESIAN_POINT('Ctrl Pts',(-0.266661635680487,0.0866348526764077,
-3.88594053764112));
#28780=CARTESIAN_POINT('Ctrl Pts',(-0.217311952916841,-0.17717095191123,
-3.87005495221662));
#28781=CARTESIAN_POINT('Ctrl Pts',(0.0311465050672407,-0.278646601116737,
-3.85416936679211));
#28782=CARTESIAN_POINT('Ctrl Pts',(0.251067394679135,-0.124816552964098,
-3.83828378136761));
#28783=CARTESIAN_POINT('Ctrl Pts',(0.240951752322899,0.143374703072453,
-3.82239819594309));
#28784=CARTESIAN_POINT('Ctrl Pts',(0.0100675354129855,0.280201172186297,
-3.80651261051859));
#28785=CARTESIAN_POINT('Ctrl Pts',(-0.230040467341084,0.160297449368488,
-3.79062702509408));
#28786=CARTESIAN_POINT('Ctrl Pts',(-0.25937826877251,-0.106476032726035,
-3.77474143966958));
#28787=CARTESIAN_POINT('Ctrl Pts',(-0.0510630698782088,-0.275693101540268,
-3.75885585424507));
#28788=CARTESIAN_POINT('Ctrl Pts',(0.204034714334676,-0.192309399147709,
-3.74297026882056));
#28789=CARTESIAN_POINT('Ctrl Pts',(0.272194945935335,0.0672725301932114,
-3.72708468339606));
#28790=CARTESIAN_POINT('Ctrl Pts',(0.0909488961210605,0.265221500669614,
-3.71119909797155));
#28791=CARTESIAN_POINT('Ctrl Pts',(-0.173604808053276,0.220156709613621,
-3.69531351254704));
#28792=CARTESIAN_POINT('Ctrl Pts',(-0.279139983968874,-0.0266066105323439,
-3.67942792712253));
#28793=CARTESIAN_POINT('Ctrl Pts',(-0.12883195646667,-0.249024285245638,
-3.66354234169802));
#28794=CARTESIAN_POINT('Ctrl Pts',(0.139350939164339,-0.243214763219636,
-3.64765675627352));
#28795=CARTESIAN_POINT('Ctrl Pts',(0.280177793680504,-0.0146860234836151,
-3.63177117084901));
#28796=CARTESIAN_POINT('Ctrl Pts',(0.163650290907218,0.227552512000709,
-3.61588558542451));
#28797=CARTESIAN_POINT('Ctrl Pts',(-0.0130164034045845,0.24961831823673,
-3.6052951951415));
#28798=CARTESIAN_POINT('Ctrl Pts',(-0.0864920085589077,0.220841828194855,
-3.6));
#28799=CARTESIAN_POINT('Ctrl Pts',(-0.112236674703446,0.230288577939269,
-5.98774893273369));
#28800=CARTESIAN_POINT('Ctrl Pts',(-0.188855278898692,0.192946659237761,
-5.98245373759219));
#28801=CARTESIAN_POINT('Ctrl Pts',(-0.300555347035098,0.0364040831712175,
-5.97186334730918));
#28802=CARTESIAN_POINT('Ctrl Pts',(-0.193285981998013,-0.233406599568089,
-5.95597776188468));
#28803=CARTESIAN_POINT('Ctrl Pts',(0.0913492619115004,-0.288663100474548,
-5.94009217646017));
#28804=CARTESIAN_POINT('Ctrl Pts',(0.292148922895039,-0.0797821279451774,
-5.92420659103567));
#28805=CARTESIAN_POINT('Ctrl Pts',(0.225342952962235,0.202375202450449,
-5.90832100561115));
#28806=CARTESIAN_POINT('Ctrl Pts',(-0.0479669356946704,0.299017834964786,
-5.89243542018666));
#28807=CARTESIAN_POINT('Ctrl Pts',(-0.277308766712869,0.121737302010726,
-5.87654983476215));
#28808=CARTESIAN_POINT('Ctrl Pts',(-0.252580570454855,-0.167107660054908,
-5.86066424933764));
#28809=CARTESIAN_POINT('Ctrl Pts',(0.00357581005461561,-0.302830118134215,
-5.84477866391314));
#28810=CARTESIAN_POINT('Ctrl Pts',(0.256453265024457,-0.161095682984698,
-5.82889307848862));
#28811=CARTESIAN_POINT('Ctrl Pts',(0.274360717694467,0.128243594027568,
-5.81300749306412));
#28812=CARTESIAN_POINT('Ctrl Pts',(0.040888662882935,0.300079889238701,
-5.79712190763961));
#28813=CARTESIAN_POINT('Ctrl Pts',(-0.230046635794548,0.196973497031616,
-5.7812363222151));
#28814=CARTESIAN_POINT('Ctrl Pts',(-0.290205422426916,-0.0866073107544878,
-5.7653507367906));
#28815=CARTESIAN_POINT('Ctrl Pts',(-0.0844678438212043,-0.290835255197635,
-5.74946515136609));
#28816=CARTESIAN_POINT('Ctrl Pts',(0.198662050370586,-0.22858998373551,
-5.73357956594158));
#28817=CARTESIAN_POINT('Ctrl Pts',(0.299770914235171,0.0430974193541643,
-5.71769398051708));
#28818=CARTESIAN_POINT('Ctrl Pts',(0.126219262205683,0.275297439287351,
-5.70180839509257));
#28819=CARTESIAN_POINT('Ctrl Pts',(-0.162978845847265,0.255260420400609,
-5.68592280966807));
#28820=CARTESIAN_POINT('Ctrl Pts',(-0.30285008978768,0.0013449474637867,
-5.67003722424355));
#28821=CARTESIAN_POINT('Ctrl Pts',(-0.165239582168466,-0.253802808289563,
-5.65415163881905));
#28822=CARTESIAN_POINT('Ctrl Pts',(0.123769157206752,-0.276407636170786,
-5.63826605339454));
#28823=CARTESIAN_POINT('Ctrl Pts',(0.299376305156942,-0.0457582056792222,
-5.62238046797004));
#28824=CARTESIAN_POINT('Ctrl Pts',(0.200684505056548,0.226816478283401,
-5.60649488254552));
#28825=CARTESIAN_POINT('Ctrl Pts',(-0.0818813945837688,0.291574043246857,
-5.59060929712102));
#28826=CARTESIAN_POINT('Ctrl Pts',(-0.28942472239694,0.0891813630520081,
-5.57472371169651));
#28827=CARTESIAN_POINT('Ctrl Pts',(-0.231787087451459,-0.194922373092896,
-5.55883812627201));
#28828=CARTESIAN_POINT('Ctrl Pts',(0.0382219112205695,-0.300431474641856,
-5.5429525408475));
#28829=CARTESIAN_POINT('Ctrl Pts',(0.2732106699911,-0.130674845520605,-5.52706695542299));
#28830=CARTESIAN_POINT('Ctrl Pts',(0.257874342861093,0.158810606515963,
-5.51118136999849));
#28831=CARTESIAN_POINT('Ctrl Pts',(0.00626460434363062,0.302788276163322,
-5.49529578457398));
#28832=CARTESIAN_POINT('Ctrl Pts',(-0.251084981819014,0.169340831915528,
-5.47941019914947));
#28833=CARTESIAN_POINT('Ctrl Pts',(-0.278381804511037,-0.119262552236759,
-5.46352461372497));
#28834=CARTESIAN_POINT('Ctrl Pts',(-0.0506155686184515,-0.298593452142671,
-5.44763902830046));
#28835=CARTESIAN_POINT('Ctrl Pts',(0.223526405683357,-0.204342681325335,
-5.43175344287595));
#28836=CARTESIAN_POINT('Ctrl Pts',(0.292865739208162,0.0771339370640931,
-5.41586785745144));
#28837=CARTESIAN_POINT('Ctrl Pts',(0.0938713311352587,0.287937768692942,
-5.39998227202694));
#28838=CARTESIAN_POINT('Ctrl Pts',(-0.191131244299241,0.234923036123716,
-5.38409668660243));
#28839=CARTESIAN_POINT('Ctrl Pts',(-0.301012748700572,-0.0333363250627414,
-5.36821110117793));
#28840=CARTESIAN_POINT('Ctrl Pts',(-0.135095939014926,-0.271051789720416,
-5.35232551575341));
#28841=CARTESIAN_POINT('Ctrl Pts',(0.15460045270224,-0.260420209417829,
-5.33643993032891));
#28842=CARTESIAN_POINT('Ctrl Pts',(0.302646550880586,-0.011182606540892,
-5.3205543449044));
#28843=CARTESIAN_POINT('Ctrl Pts',(0.173397388783639,0.248300888061197,
-5.3046687594799));
#28844=CARTESIAN_POINT('Ctrl Pts',(-0.114724471230777,0.280282502396747,
-5.28878317405539));
#28845=CARTESIAN_POINT('Ctrl Pts',(-0.29773179411493,0.0554595728623016,
-5.27289758863089));
#28846=CARTESIAN_POINT('Ctrl Pts',(-0.207946927228169,-0.220177339672652,
-5.25701200320637));
#28847=CARTESIAN_POINT('Ctrl Pts',(0.0723661222577529,-0.294080141795293,
-5.24112641778187));
#28848=CARTESIAN_POINT('Ctrl Pts',(0.286374822170912,-0.0985365245761303,
-5.22524083235736));
#28849=CARTESIAN_POINT('Ctrl Pts',(0.237996983664519,0.187289671940431,
-5.20935524693285));
#28850=CARTESIAN_POINT('Ctrl Pts',(-0.0284419407454325,0.301514579175862,
-5.19346966150835));
#28851=CARTESIAN_POINT('Ctrl Pts',(-0.268821373187637,0.13948137784836,
-5.17758407608384));
#28852=CARTESIAN_POINT('Ctrl Pts',(-0.262897345607792,-0.150349496578276,
-5.16169849065933));
#28853=CARTESIAN_POINT('Ctrl Pts',(-0.0160976574136605,-0.302424950813844,
-5.14581290523482));
#28854=CARTESIAN_POINT('Ctrl Pts',(0.245451262481131,-0.177408182436388,
-5.12992731981032));
#28855=CARTESIAN_POINT('Ctrl Pts',(0.282109227839787,0.110156112025631,
-5.11404173438581));
#28856=CARTESIAN_POINT('Ctrl Pts',(0.0602889401594312,0.296791558409967,
-5.09815614896131));
#28857=CARTESIAN_POINT('Ctrl Pts',(-0.21677016423497,0.211496291566797,
-5.0822705635368));
#28858=CARTESIAN_POINT('Ctrl Pts',(-0.295216930452845,-0.0675792085109285,
-5.06638497811229));
#28859=CARTESIAN_POINT('Ctrl Pts',(-0.103175712157411,-0.284736295315112,
-5.05049939268779));
#28860=CARTESIAN_POINT('Ctrl Pts',(0.183398669901276,-0.241008118799775,
-5.03461380726328));
#28861=CARTESIAN_POINT('Ctrl Pts',(0.301936833617324,0.0235400500022461,
-5.01872822183878));
#28862=CARTESIAN_POINT('Ctrl Pts',(0.143830004614954,0.266520009045148,
-5.00284263641426));
#28863=CARTESIAN_POINT('Ctrl Pts',(-0.146058860062545,0.265305097663414,
-4.98695705098977));
#28864=CARTESIAN_POINT('Ctrl Pts',(-0.302123534447069,0.0210084597763427,
-4.97107146556525));
#28865=CARTESIAN_POINT('Ctrl Pts',(-0.181372154341526,-0.242536857154696,
-4.95518588014075));
#28866=CARTESIAN_POINT('Ctrl Pts',(0.105558680307571,-0.283861498729024,
-4.93930029471624));
#28867=CARTESIAN_POINT('Ctrl Pts',(0.295772993175611,-0.0651023959382731,
-4.92341470929173));
#28868=CARTESIAN_POINT('Ctrl Pts',(0.214989837589453,0.213305778595482,
-4.90752912386722));
#28869=CARTESIAN_POINT('Ctrl Pts',(-0.0627744591907873,0.296275805158416,
-4.89164353844272));
#28870=CARTESIAN_POINT('Ctrl Pts',(-0.283022620567196,0.107787669499998,
-4.87575795301821));
#28871=CARTESIAN_POINT('Ctrl Pts',(-0.243955646827653,-0.179459265098978,
-4.8598723675937));
#28872=CARTESIAN_POINT('Ctrl Pts',(0.0186319465451625,-0.302279400583139,
-4.8439867821692));
#28873=CARTESIAN_POINT('Ctrl Pts',(0.264148304671307,-0.148140671620721,
-4.82810119674469));
#28874=CARTESIAN_POINT('Ctrl Pts',(0.267642830128331,0.141729675544189,
-4.81221561132019));
#28875=CARTESIAN_POINT('Ctrl Pts',(0.025913717564994,0.301742381330375,
-4.79633002589567));
#28876=CARTESIAN_POINT('Ctrl Pts',(-0.239558441254702,0.185288258323568,
-4.78044444047117));
#28877=CARTESIAN_POINT('Ctrl Pts',(-0.285538852603348,-0.100933389435444,
-4.76455885504666));
#28878=CARTESIAN_POINT('Ctrl Pts',(-0.069898669826687,-0.294676367232637,
-4.74867326962215));
#28879=CARTESIAN_POINT('Ctrl Pts',(0.209785097078365,-0.218426643275917,
-4.73278768419765));
#28880=CARTESIAN_POINT('Ctrl Pts',(0.297256486452718,0.0579531423716499,
-4.71690209877314));
#28881=CARTESIAN_POINT('Ctrl Pts',(0.112371179411428,0.281234250201941,
-4.70101651334864));
#28882=CARTESIAN_POINT('Ctrl Pts',(-0.175472497225253,0.246838789833562,
-4.68513092792412));
#28883=CARTESIAN_POINT('Ctrl Pts',(-0.302542189662687,-0.0137189257258342,
-4.66924534249962));
#28884=CARTESIAN_POINT('Ctrl Pts',(-0.152412241190043,-0.261706886008741,
-4.65335975707511));
#28885=CARTESIAN_POINT('Ctrl Pts',(0.137363085585984,-0.269909926025816,
-4.63747417165061));
#28886=CARTESIAN_POINT('Ctrl Pts',(0.301281592058078,-0.0308121361789995,
-4.6215885862261));
#28887=CARTESIAN_POINT('Ctrl Pts',(0.189155460840372,0.236516800847699,
-4.60570300080159));
#28888=CARTESIAN_POINT('Ctrl Pts',(-0.0962814601207137,0.287140846773822,
-4.58981741537709));
#28889=CARTESIAN_POINT('Ctrl Pts',(-0.293501970003673,0.0746764959872007,
-4.57393182995257));
#28890=CARTESIAN_POINT('Ctrl Pts',(-0.221805801580948,-0.206209048865458,
-4.55804624452808));
#28891=CARTESIAN_POINT('Ctrl Pts',(0.0531165305003444,-0.298158715513348,
-4.54216065910356));
#28892=CARTESIAN_POINT('Ctrl Pts',(0.279371656207873,-0.116925032207111,
-4.52627507367906));
#28893=CARTESIAN_POINT('Ctrl Pts',(0.249656786895474,0.171439418471925,
-4.51038948825455));
#28894=CARTESIAN_POINT('Ctrl Pts',(-0.00880228419370061,0.302725131500404,
-4.49450390283004));
#28895=CARTESIAN_POINT('Ctrl Pts',(-0.259196397399141,0.156643585965945,
-4.47861831740554));
#28896=CARTESIAN_POINT('Ctrl Pts',(-0.272105787021618,-0.132960242622783,
-4.46273273198103));
#28897=CARTESIAN_POINT('Ctrl Pts',(-0.035702422822744,-0.300741288242153,
-4.44684714655653));
#28898=CARTESIAN_POINT('Ctrl Pts',(0.233412738686511,-0.192972741255926,
-4.43096156113201));
#28899=CARTESIAN_POINT('Ctrl Pts',(0.288667058440516,0.0916041201052846,
-4.41507597570751));
#28900=CARTESIAN_POINT('Ctrl Pts',(0.0794346134510843,0.292250111436831,
-4.399190390283));
#28901=CARTESIAN_POINT('Ctrl Pts',(-0.202578577751036,0.225126420673654,
-4.3833048048585));
#28902=CARTESIAN_POINT('Ctrl Pts',(-0.298982254223097,-0.0482659000603877,
-4.36741921943399));
#28903=CARTESIAN_POINT('Ctrl Pts',(-0.121448026029594,-0.277435330162687,
-4.35153363400948));
#28904=CARTESIAN_POINT('Ctrl Pts',(0.167361093253233,-0.252408894284742,
-4.33564804858498));
#28905=CARTESIAN_POINT('Ctrl Pts',(0.302828177814098,0.00388331955378666,
-4.31976246316047));
#28906=CARTESIAN_POINT('Ctrl Pts',(0.16083358920762,0.256617501413209,-4.30387687773596));
#28907=CARTESIAN_POINT('Ctrl Pts',(-0.128522308657371,0.274229833581875,
-4.28799129231146));
#28908=CARTESIAN_POINT('Ctrl Pts',(-0.30012161248013,0.0405832868468127,
-4.27210570688694));
#28909=CARTESIAN_POINT('Ctrl Pts',(-0.196739092109704,-0.230247073998374,
-4.25622012146245));
#28910=CARTESIAN_POINT('Ctrl Pts',(0.0869026038374818,-0.290117084804099,
-4.24033453603793));
#28911=CARTESIAN_POINT('Ctrl Pts',(0.290921121923897,-0.0841717664511477,
-4.22444895061343));
#28912=CARTESIAN_POINT('Ctrl Pts',(0.228387624172868,0.198894641892724,
-4.20856336518892));
#28913=CARTESIAN_POINT('Ctrl Pts',(-0.0434025312350796,0.299726885232788,
-4.19267777976441));
#28914=CARTESIAN_POINT('Ctrl Pts',(-0.275425783103537,0.125938967165763,
-4.17679219433991));
#28915=CARTESIAN_POINT('Ctrl Pts',(-0.255094385662357,-0.163238597924922,
-4.1609066089154));
#28916=CARTESIAN_POINT('Ctrl Pts',(-0.00103666997583505,-0.302851301407654,
-4.1450210234909));
#28917=CARTESIAN_POINT('Ctrl Pts',(0.253970878675925,-0.164981145085206,
-4.12913543806639));
#28918=CARTESIAN_POINT('Ctrl Pts',(0.276281505125808,0.124050454953884,
-4.11324985264188));
#28919=CARTESIAN_POINT('Ctrl Pts',(0.0454534400891082,0.299422728317279,
-4.09736426721737));
#28920=CARTESIAN_POINT('Ctrl Pts',(-0.227020642269675,0.200453519382929,
-4.08147868179287));
#28921=CARTESIAN_POINT('Ctrl Pts',(-0.291490543170309,-0.0821781521469477,
-4.06559309636836));
#28922=CARTESIAN_POINT('Ctrl Pts',(-0.0888867047566989,-0.289515352211788,
-4.04970751094385));
#28923=CARTESIAN_POINT('Ctrl Pts',(0.19515821356546,-0.231588551381047,
-4.03382192551934));
#28924=CARTESIAN_POINT('Ctrl Pts',(0.300392412005423,0.0385277075746812,
-4.01793634009484));
#28925=CARTESIAN_POINT('Ctrl Pts',(0.130396670387433,0.273343545382419,
-4.00205075467033));
#28926=CARTESIAN_POINT('Ctrl Pts',(-0.159073020549541,0.257712552289462,
-3.98616516924583));
#28927=CARTESIAN_POINT('Ctrl Pts',(-0.302794496082807,0.00595638587028517,
-3.97027958382131));
#28928=CARTESIAN_POINT('Ctrl Pts',(-0.169085159156036,-0.251257227616604,
-3.95439399839681));
#28929=CARTESIAN_POINT('Ctrl Pts',(0.119545862085038,-0.278260260309545,
-3.9385084129723));
#28930=CARTESIAN_POINT('Ctrl Pts',(0.298644819514743,-0.0503115969522353,
-3.9226228275478));
#28931=CARTESIAN_POINT('Ctrl Pts',(0.204115044091895,0.223734294517963,
-3.90673724212329));
#28932=CARTESIAN_POINT('Ctrl Pts',(-0.0774320144894472,0.292787072031722,
-3.89085165669878));
#28933=CARTESIAN_POINT('Ctrl Pts',(-0.288033168338763,0.0935781821080819,
-3.87496607127428));
#28934=CARTESIAN_POINT('Ctrl Pts',(-0.234728367118847,-0.191370275241736,
-3.85908048584977));
#28935=CARTESIAN_POINT('Ctrl Pts',(0.0336427342249789,-0.300978665947462,
-3.84319490042527));
#28936=CARTESIAN_POINT('Ctrl Pts',(0.271189130642844,-0.134819945582456,
-3.82730931500076));
#28937=CARTESIAN_POINT('Ctrl Pts',(0.260262772562825,0.154865434167926,
-3.81142372957625));
#28938=CARTESIAN_POINT('Ctrl Pts',(0.0108743956173709,0.302657827741511,
-3.79553814415174));
#28939=CARTESIAN_POINT('Ctrl Pts',(-0.248477005270357,0.173144449895859,
-3.77965255872723));
#28940=CARTESIAN_POINT('Ctrl Pts',(-0.280166077741629,-0.115009528760893,
-3.76376697330273));
#28941=CARTESIAN_POINT('Ctrl Pts',(-0.0551555073326973,-0.297788458857768,
-3.74788138787822));
#28942=CARTESIAN_POINT('Ctrl Pts',(0.220387027443752,-0.207721989691116,
-3.73199580245372));
#28943=CARTESIAN_POINT('Ctrl Pts',(0.294009944413199,0.0726640709461968,
-3.71611021702921));
#28944=CARTESIAN_POINT('Ctrl Pts',(0.0982379735270597,0.286477614053803,
-3.7002246316047));
#28945=CARTESIAN_POINT('Ctrl Pts',(-0.18751832364196,0.237801116156914,
-3.68433904618019));
#28946=CARTESIAN_POINT('Ctrl Pts',(-0.301511590849623,-0.0287389909344478,
-3.66845346075569));
#28947=CARTESIAN_POINT('Ctrl Pts',(-0.139157162633019,-0.268982276695176,
-3.65256787533117));
#28948=CARTESIAN_POINT('Ctrl Pts',(0.15051918666913,-0.262707151923616,
-3.63668228990668));
#28949=CARTESIAN_POINT('Ctrl Pts',(0.302632575570994,-0.0158630313036537,
-3.62079670448216));
#28950=CARTESIAN_POINT('Ctrl Pts',(0.176766004113337,0.245789653347592,
-3.60491111905766));
#28951=CARTESIAN_POINT('Ctrl Pts',(-0.0140595999249409,0.269623918317471,
-3.59432072877466));
#28952=CARTESIAN_POINT('Ctrl Pts',(-0.0934238897831399,0.238541143402067,
-3.58902553363315));
#28953=CARTESIAN_POINT('Ctrl Pts',(-0.120564430054385,0.247375567929493,
-5.97677446636685));
#28954=CARTESIAN_POINT('Ctrl Pts',(-0.202867994114616,0.2072629473687,-5.97147927122534));
#28955=CARTESIAN_POINT('Ctrl Pts',(-0.322856002379157,0.0391051993547299,
-5.96088888094234));
#28956=CARTESIAN_POINT('Ctrl Pts',(-0.207627447255233,-0.250724941042775,
-5.94500329551783));
#28957=CARTESIAN_POINT('Ctrl Pts',(0.0981272095538185,-0.31008137294161,
-5.92911771009333));
#28958=CARTESIAN_POINT('Ctrl Pts',(0.31382583699053,-0.0857018154685313,
-5.91323212466882));
#28959=CARTESIAN_POINT('Ctrl Pts',(0.242062986652523,0.217391071189942,
-5.89734653924431));
#28960=CARTESIAN_POINT('Ctrl Pts',(-0.0515259943219408,0.321204409733984,
-5.88146095381981));
#28961=CARTESIAN_POINT('Ctrl Pts',(-0.297884568445745,0.13076998647779,
-5.8655753683953));
#28962=CARTESIAN_POINT('Ctrl Pts',(-0.271321585392319,-0.179506741851318,
-5.84968978297079));
#28963=CARTESIAN_POINT('Ctrl Pts',(0.0038411286004027,-0.32529955732048,
-5.83380419754628));
#28964=CARTESIAN_POINT('Ctrl Pts',(0.275481626794049,-0.173048687112214,
-5.81791861212178));
#28965=CARTESIAN_POINT('Ctrl Pts',(0.294717779598738,0.137759033425684,
-5.80203302669727));
#28966=CARTESIAN_POINT('Ctrl Pts',(0.0439225266535408,0.322345266486553,
-5.78614744127277));
#28967=CARTESIAN_POINT('Ctrl Pts',(-0.247115674121507,0.211588569139127,
-5.77026185584825));
#28968=CARTESIAN_POINT('Ctrl Pts',(-0.311738132353264,-0.093033414320651,
-5.75437627042376));
#28969=CARTESIAN_POINT('Ctrl Pts',(-0.0907352028660341,-0.312414697560065,
-5.73849068499924));
#28970=CARTESIAN_POINT('Ctrl Pts',(0.21340241003799,-0.245550941152097,
-5.72260509957474));
#28971=CARTESIAN_POINT('Ctrl Pts',(0.322013366104615,0.046295168802699,
-5.70671951415023));
#28972=CARTESIAN_POINT('Ctrl Pts',(0.135584499896502,0.295724004215282,
-5.69083392872572));
#28973=CARTESIAN_POINT('Ctrl Pts',(-0.175071577204289,0.274200275287532,
-5.67494834330122));
#28974=CARTESIAN_POINT('Ctrl Pts',(-0.325321010833992,0.00144474009812678,
-5.6590627578767));
#28975=CARTESIAN_POINT('Ctrl Pts',(-0.177500056012922,-0.272634511032016,
-5.64317717245221));
#28976=CARTESIAN_POINT('Ctrl Pts',(0.132952601601671,-0.296916575670675,
-5.62729158702769));
#28977=CARTESIAN_POINT('Ctrl Pts',(0.321589477756739,-0.049153380591534,
-5.61140600160319));
#28978=CARTESIAN_POINT('Ctrl Pts',(0.215574927151207,0.243645844849156,
-5.59552041617868));
#28979=CARTESIAN_POINT('Ctrl Pts',(-0.0879568438403424,0.313208302327141,
-5.57963483075418));
#28980=CARTESIAN_POINT('Ctrl Pts',(-0.310899505813355,0.0957984565762295,
-5.56374924532966));
#28981=CARTESIAN_POINT('Ctrl Pts',(-0.248985264098286,-0.209385255567195,
-5.54786365990517));
#28982=CARTESIAN_POINT('Ctrl Pts',(0.0410579069103138,-0.322722938881596,
-5.53197807448065));
#28983=CARTESIAN_POINT('Ctrl Pts',(0.293482400465685,-0.140370679319073,
-5.51609248905615));
#28984=CARTESIAN_POINT('Ctrl Pts',(0.27700814599902,0.170594062161754,-5.50020690363163));
#28985=CARTESIAN_POINT('Ctrl Pts',(0.0067294264927366,0.32525461075211,
-5.48432131820714));
#28986=CARTESIAN_POINT('Ctrl Pts',(-0.269715026823541,0.181905610966966,
-5.46843573278263));
#28987=CARTESIAN_POINT('Ctrl Pts',(-0.299037223679916,-0.128111614810828,
-5.45255014735812));
#28988=CARTESIAN_POINT('Ctrl Pts',(-0.0543711509494218,-0.320748538485051,
-5.43666456193362));
#28989=CARTESIAN_POINT('Ctrl Pts',(0.240111654898234,-0.219504533387761,
-5.4207789765091));
#28990=CARTESIAN_POINT('Ctrl Pts',(0.314595839758998,0.0828571336825043,
-5.4048933910846));
#28991=CARTESIAN_POINT('Ctrl Pts',(0.100836411686931,0.30930222287252,-5.38900780566009));
#28992=CARTESIAN_POINT('Ctrl Pts',(-0.205312831972345,0.252353894408739,
-5.37312222023558));
#28993=CARTESIAN_POINT('Ctrl Pts',(-0.323347342409049,-0.0358098192227868,
-5.35723663481108));
#28994=CARTESIAN_POINT('Ctrl Pts',(-0.145119809839629,-0.29116333523965,
-5.34135104938657));
#28995=CARTESIAN_POINT('Ctrl Pts',(0.166071522659101,-0.279742911183559,
-5.32546546396207));
#28996=CARTESIAN_POINT('Ctrl Pts',(0.325102369713409,-0.0120123354303517,
-5.30957987853755));
#28997=CARTESIAN_POINT('Ctrl Pts',(0.186263156912436,0.266724358416659,
-5.29369429311305));
#28998=CARTESIAN_POINT('Ctrl Pts',(-0.123236816519873,0.30107894986168,
-5.27780870768855));
#28999=CARTESIAN_POINT('Ctrl Pts',(-0.319822947012469,0.0595745714212406,
-5.26192312226403));
#29000=CARTESIAN_POINT('Ctrl Pts',(-0.22337620772415,-0.23651409433381,
-5.24603753683954));
#29001=CARTESIAN_POINT('Ctrl Pts',(0.0777355557646795,-0.315900348790123,
-5.23015195141502));
#29002=CARTESIAN_POINT('Ctrl Pts',(0.307623308585974,-0.105847753922241,
-5.21426636599052));
#29003=CARTESIAN_POINT('Ctrl Pts',(0.255655923217533,0.201186221992351,
-5.198380780566));
#29004=CARTESIAN_POINT('Ctrl Pts',(-0.0305522805684868,0.323886407784935,
-5.1824951951415));
#29005=CARTESIAN_POINT('Ctrl Pts',(-0.288767425892113,0.149830640188875,
-5.166609609717));
#29006=CARTESIAN_POINT('Ctrl Pts',(-0.282403846334204,-0.161505153389643,
-5.15072402429249));
#29007=CARTESIAN_POINT('Ctrl Pts',(-0.0172920740606111,-0.324864327328267,
-5.13483843886798));
#29008=CARTESIAN_POINT('Ctrl Pts',(0.263663295846542,-0.190571544095922,
-5.11895285344348));
#29009=CARTESIAN_POINT('Ctrl Pts',(0.30304121498124,0.118329493442925,-5.10306726801897));
#29010=CARTESIAN_POINT('Ctrl Pts',(0.0647622689117458,0.318812947543176,
-5.08718168259446));
#29011=CARTESIAN_POINT('Ctrl Pts',(-0.232854112729537,0.227188928384957,
-5.07129609716995));
#29012=CARTESIAN_POINT('Ctrl Pts',(-0.317121485080486,-0.072593461800026,
-5.05541051174545));
#29013=CARTESIAN_POINT('Ctrl Pts',(-0.11083116071089,-0.305863206043554,
-5.03952492632094));
#29014=CARTESIAN_POINT('Ctrl Pts',(0.197006514740415,-0.258890479055526,
-5.02363934089643));
#29015=CARTESIAN_POINT('Ctrl Pts',(0.324339992731277,0.0252866785252807,
-5.00775375547193));
#29016=CARTESIAN_POINT('Ctrl Pts',(0.154501927083457,0.286295304752389,
-4.99186817004741));
#29017=CARTESIAN_POINT('Ctrl Pts',(-0.156896159516148,0.284990249175035,
-4.97598258462292));
#29018=CARTESIAN_POINT('Ctrl Pts',(-0.324540546420063,0.0225672489491302,
-4.9600969991984));
#29019=CARTESIAN_POINT('Ctrl Pts',(-0.194829635444025,-0.260532646991722,
-4.9442114137739));
#29020=CARTESIAN_POINT('Ctrl Pts',(0.113390940725942,-0.304923501155701,
-4.92832582834939));
#29021=CARTESIAN_POINT('Ctrl Pts',(0.317718806637116,-0.0699328742784981,
-4.91244024292489));
#29022=CARTESIAN_POINT('Ctrl Pts',(0.230941689113151,0.229132676031443,
-4.89655465750038));
#29023=CARTESIAN_POINT('Ctrl Pts',(-0.0674322088952368,0.318258926346574,
-4.88066907207587));
#29024=CARTESIAN_POINT('Ctrl Pts',(-0.304022379773291,0.115785316827091,
-4.86478348665136));
#29025=CARTESIAN_POINT('Ctrl Pts',(-0.262056708255467,-0.192774813329111,
-4.84889790122685));
#29026=CARTESIAN_POINT('Ctrl Pts',(0.020014402796204,-0.324707977537473,
-4.83301231580236));
#29027=CARTESIAN_POINT('Ctrl Pts',(0.283747624265194,-0.1591324376726,-4.81712673037784));
#29028=CARTESIAN_POINT('Ctrl Pts',(0.287501437099989,0.152245757448955,
-4.80124114495334));
#29029=CARTESIAN_POINT('Ctrl Pts',(0.0278364678663976,0.324131112441382,
-4.78535555952883));
#29030=CARTESIAN_POINT('Ctrl Pts',(-0.257333238096221,0.199036307156957,
-4.76946997410432));
#29031=CARTESIAN_POINT('Ctrl Pts',(-0.306725311610187,-0.108422461756772,
-4.75358438867982));
#29032=CARTESIAN_POINT('Ctrl Pts',(-0.0750850228900749,-0.316540813061068,
-4.73769880325531));
#29033=CARTESIAN_POINT('Ctrl Pts',(0.225350766404881,-0.234633499476306,
-4.7218132178308));
#29034=CARTESIAN_POINT('Ctrl Pts',(0.319312372393732,0.0622531592134212,
-4.7059276324063));
#29035=CARTESIAN_POINT('Ctrl Pts',(0.120708914764934,0.302101315607921,
-4.69004204698178));
#29036=CARTESIAN_POINT('Ctrl Pts',(-0.188492234593375,0.265153775182933,
-4.67415646155729));
#29037=CARTESIAN_POINT('Ctrl Pts',(-0.324990265084604,-0.0147368448456257,
-4.65827087613277));
#29038=CARTESIAN_POINT('Ctrl Pts',(-0.163720949867243,-0.281125056816949,
-4.64238529070827));
#29039=CARTESIAN_POINT('Ctrl Pts',(0.1475551745269,-0.2899367473538,-4.62649970528376));
#29040=CARTESIAN_POINT('Ctrl Pts',(0.323636133450456,-0.0330983401548074,
-4.61061411985925));
#29041=CARTESIAN_POINT('Ctrl Pts',(0.203190449005647,0.254065913551284,
-4.59472853443475));
#29042=CARTESIAN_POINT('Ctrl Pts',(-0.103425367821428,0.308446170809053,
-4.57884294901024));
#29043=CARTESIAN_POINT('Ctrl Pts',(-0.315279277712293,0.0802173549861858,
-4.56295736358573));
#29044=CARTESIAN_POINT('Ctrl Pts',(-0.238263385128086,-0.221509381975279,
-4.54707177816123));
#29045=CARTESIAN_POINT('Ctrl Pts',(0.0570576796146275,-0.32028154519541,
-4.53118619273672));
#29046=CARTESIAN_POINT('Ctrl Pts',(0.300100520556651,-0.12560065508345,
-4.51530060731221));
#29047=CARTESIAN_POINT('Ctrl Pts',(0.268180862456874,0.184159908795732,
-4.4994150218877));
#29048=CARTESIAN_POINT('Ctrl Pts',(-0.00945539753199466,0.325186780871051,
-4.4835294364632));
#29049=CARTESIAN_POINT('Ctrl Pts',(-0.278428294558318,0.168266252662592,
-4.46764385103869));
#29050=CARTESIAN_POINT('Ctrl Pts',(-0.292295537206912,-0.142825648693389,
-4.45175826561419));
#29051=CARTESIAN_POINT('Ctrl Pts',(-0.0383514770956826,-0.323055740082643,
-4.43587268018968));
#29052=CARTESIAN_POINT('Ctrl Pts',(0.250731535672522,-0.207290964624762,
-4.41998709476517));
#29053=CARTESIAN_POINT('Ctrl Pts',(0.310085624581392,0.0984009777580124,
-4.40410150934067));
#29054=CARTESIAN_POINT('Ctrl Pts',(0.0853285160365348,0.313934533536481,
-4.38821592391616));
#29055=CARTESIAN_POINT('Ctrl Pts',(-0.217609536564715,0.241830388065385,
-4.37233033849165));
#29056=CARTESIAN_POINT('Ctrl Pts',(-0.321166188966538,-0.0518471412951069,
-4.35644475306714));
#29057=CARTESIAN_POINT('Ctrl Pts',(-0.13045924674957,-0.298020522671343,
-4.34055916764264));
#29058=CARTESIAN_POINT('Ctrl Pts',(0.179778979328005,-0.271137171165345,
-4.32467358221813));
#29059=CARTESIAN_POINT('Ctrl Pts',(0.325297473032169,0.00417145474024782,
-4.30878799679362));
#29060=CARTESIAN_POINT('Ctrl Pts',(0.17276714645772,0.275658049221534,-4.29290241136911));
#29061=CARTESIAN_POINT('Ctrl Pts',(-0.138058428169682,0.294577184125114,
-4.27701682594462));
#29062=CARTESIAN_POINT('Ctrl Pts',(-0.322390085515951,0.0435944922757886,
-4.2611312405201));
#29063=CARTESIAN_POINT('Ctrl Pts',(-0.211336771802054,-0.247330984472329,
-4.2452456550956));
#29064=CARTESIAN_POINT('Ctrl Pts',(0.0933506176086514,-0.3116432402409,
-4.22936006967109));
#29065=CARTESIAN_POINT('Ctrl Pts',(0.312506935439882,-0.0904171570983101,
-4.21347448424658));
#29066=CARTESIAN_POINT('Ctrl Pts',(0.24533356688116,0.213652259424352,-4.19758889882208));
#29067=CARTESIAN_POINT('Ctrl Pts',(-0.0466229194254129,0.321966070231031,
-4.18170331339757));
#29068=CARTESIAN_POINT('Ctrl Pts',(-0.295861870907166,0.135283407478856,
-4.16581772797306));
#29069=CARTESIAN_POINT('Ctrl Pts',(-0.274021921076313,-0.17535060240956,
-4.14993214254855));
#29070=CARTESIAN_POINT('Ctrl Pts',(-0.00111358898614249,-0.325322312353944,
-4.13404655712405));
#29071=CARTESIAN_POINT('Ctrl Pts',(0.2728150519327,-0.177222443372218,-4.11816097169954));
#29072=CARTESIAN_POINT('Ctrl Pts',(0.296781085933562,0.133254771125564,
-4.10227538627503));
#29073=CARTESIAN_POINT('Ctrl Pts',(0.0488260019537641,0.321639345430405,
-4.08638980085053));
#29074=CARTESIAN_POINT('Ctrl Pts',(-0.243865157428648,0.215326802764376,
-4.07050421542601));
#29075=CARTESIAN_POINT('Ctrl Pts',(-0.313118606698104,-0.0882756202702708,
-4.05461863000152));
#29076=CARTESIAN_POINT('Ctrl Pts',(-0.0954819351759957,-0.310996860194193,
-4.038733044577));
#29077=CARTESIAN_POINT('Ctrl Pts',(0.209638594970145,-0.24877199701569,
-4.0228474591525));
#29078=CARTESIAN_POINT('Ctrl Pts',(0.322680977869204,0.0413863927928797,
-4.00696187372799));
#29079=CARTESIAN_POINT('Ctrl Pts',(0.140071864101366,0.293625134967264,
-3.99107628830348));
#29080=CARTESIAN_POINT('Ctrl Pts',(-0.170875946835193,0.276834350863799,
-3.97519070287898));
#29081=CARTESIAN_POINT('Ctrl Pts',(-0.32526129217821,0.00639833877413384,
-3.95930511745447));
#29082=CARTESIAN_POINT('Ctrl Pts',(-0.181630967757783,-0.269900052943306,
-3.94341953202997));
#29083=CARTESIAN_POINT('Ctrl Pts',(0.128415945730084,-0.298906661121661,
-3.92753394660546));
#29084=CARTESIAN_POINT('Ctrl Pts',(0.320803717221891,-0.0540446251432457,
-3.91164836118095));
#29085=CARTESIAN_POINT('Ctrl Pts',(0.219260005889228,0.24033496870297,-3.89576277575645));
#29086=CARTESIAN_POINT('Ctrl Pts',(-0.0831773279059596,0.314511335622391,
-3.87987719033193));
#29087=CARTESIAN_POINT('Ctrl Pts',(-0.309404700997039,0.100521511539756,
-3.86399160490743));
#29088=CARTESIAN_POINT('Ctrl Pts',(-0.252144781320854,-0.205569598572242,
-3.84810601948292));
#29089=CARTESIAN_POINT('Ctrl Pts',(0.0361389633827169,-0.323310730778187,
-3.83222043405842));
#29090=CARTESIAN_POINT('Ctrl Pts',(0.291310866606552,-0.144823338200814,
-3.81633484863391));
#29091=CARTESIAN_POINT('Ctrl Pts',(0.279573792802751,0.1663561652634,-3.8004492632094));
#29092=CARTESIAN_POINT('Ctrl Pts',(0.0116812558217563,0.325114483296725,
-3.7845636777849));
#29093=CARTESIAN_POINT('Ctrl Pts',(-0.266913543199629,0.185991450423231,
-3.76867809236039));
#29094=CARTESIAN_POINT('Ctrl Pts',(-0.300953886710748,-0.123543024795751,
-3.75279250693588));
#29095=CARTESIAN_POINT('Ctrl Pts',(-0.0592479447871856,-0.319883816175267,
-3.73690692151138));
#29096=CARTESIAN_POINT('Ctrl Pts',(0.236739340552828,-0.223134580234524,
-3.72102133608687));
#29097=CARTESIAN_POINT('Ctrl Pts',(0.315824942891063,0.0780556116991824,
-3.70513575066236));
#29098=CARTESIAN_POINT('Ctrl Pts',(0.105527050933059,0.307733727437991,
-3.68925016523785));
#29099=CARTESIAN_POINT('Ctrl Pts',(-0.201431839230644,0.255445522700207,
-3.67336457981334));
#29100=CARTESIAN_POINT('Ctrl Pts',(-0.323883197730372,-0.0308713713365518,
-3.65747899438885));
#29101=CARTESIAN_POINT('Ctrl Pts',(-0.149482368799369,-0.288940268144714,
-3.64159340896433));
#29102=CARTESIAN_POINT('Ctrl Pts',(0.161687434173921,-0.282199540627596,
-3.62570782353983));
#29103=CARTESIAN_POINT('Ctrl Pts',(0.325087357461483,-0.0170400391236926,
-3.60982223811532));
#29104=CARTESIAN_POINT('Ctrl Pts',(0.189881717319456,0.264026794694474,
-3.59393665269081));
#29105=CARTESIAN_POINT('Ctrl Pts',(-0.0151027964452971,0.289629518398212,
-3.58334626240781));
#29106=CARTESIAN_POINT('Ctrl Pts',(-0.100355771007372,0.256240458609279,
-3.57805106726631));
#29107=CARTESIAN_POINT('Ctrl Pts',(-0.128892185405323,0.264462557919717,
-5.9658));
#29108=CARTESIAN_POINT('Ctrl Pts',(-0.216880709330539,0.22157923549964,
-5.9605048048585));
#29109=CARTESIAN_POINT('Ctrl Pts',(-0.345156657723216,0.0418063155382426,
-5.94991441457549));
#29110=CARTESIAN_POINT('Ctrl Pts',(-0.221968912512454,-0.268043282517462,
-5.93402882915099));
#29111=CARTESIAN_POINT('Ctrl Pts',(0.104905157196136,-0.331499645408673,
-5.91814324372647));
#29112=CARTESIAN_POINT('Ctrl Pts',(0.335502751086021,-0.0916215029918852,
-5.90225765830198));
#29113=CARTESIAN_POINT('Ctrl Pts',(0.258783020342812,0.232406939929434,
-5.88637207287745));
#29114=CARTESIAN_POINT('Ctrl Pts',(-0.0550850529492111,0.343390984503182,
-5.87048648745297));
#29115=CARTESIAN_POINT('Ctrl Pts',(-0.318460370178621,0.139802670944853,
-5.85460090202845));
#29116=CARTESIAN_POINT('Ctrl Pts',(-0.290062600329783,-0.191905823647729,
-5.83871531660395));
#29117=CARTESIAN_POINT('Ctrl Pts',(0.00410644714618952,-0.347768996506744,
-5.82282973117944));
#29118=CARTESIAN_POINT('Ctrl Pts',(0.294509988563641,-0.18500169123973,
-5.80694414575493));
#29119=CARTESIAN_POINT('Ctrl Pts',(0.315074841503008,0.1472744728238,-5.79105856033042));
#29120=CARTESIAN_POINT('Ctrl Pts',(0.046956390424147,0.344610643734406,
-5.77517297490592));
#29121=CARTESIAN_POINT('Ctrl Pts',(-0.264184712448466,0.226203641246638,
-5.75928738948141));
#29122=CARTESIAN_POINT('Ctrl Pts',(-0.333270842279612,-0.0994595178868144,
-5.7434018040569));
#29123=CARTESIAN_POINT('Ctrl Pts',(-0.097002561910864,-0.333994139922494,
-5.7275162186324));
#29124=CARTESIAN_POINT('Ctrl Pts',(0.228142769705393,-0.262511898568683,
-5.71163063320788));
#29125=CARTESIAN_POINT('Ctrl Pts',(0.344255817974058,0.0494929182512338,
-5.69574504778339));
#29126=CARTESIAN_POINT('Ctrl Pts',(0.144949737587321,0.316150569143213,
-5.67985946235887));
#29127=CARTESIAN_POINT('Ctrl Pts',(-0.187164308561312,0.293140130174455,
-5.66397387693438));
#29128=CARTESIAN_POINT('Ctrl Pts',(-0.347791931880303,0.00154453273246722,
-5.64808829150985));
#29129=CARTESIAN_POINT('Ctrl Pts',(-0.189760529857378,-0.291466213774469,
-5.63220270608536));
#29130=CARTESIAN_POINT('Ctrl Pts',(0.14213604599659,-0.317425515170563,
-5.61631712066084));
#29131=CARTESIAN_POINT('Ctrl Pts',(0.343802650356538,-0.0525485555038461,
-5.60043153523635));
#29132=CARTESIAN_POINT('Ctrl Pts',(0.230465349245865,0.260475211414911,
-5.58454594981184));
#29133=CARTESIAN_POINT('Ctrl Pts',(-0.0940322930969158,0.334842561407425,
-5.56866036438732));
#29134=CARTESIAN_POINT('Ctrl Pts',(-0.33237428922977,0.102415550100451,
-5.55277477896283));
#29135=CARTESIAN_POINT('Ctrl Pts',(-0.266183440745114,-0.223848138041494,
-5.53688919353831));
#29136=CARTESIAN_POINT('Ctrl Pts',(0.0438939026000584,-0.345014403121335,
-5.52100360811381));
#29137=CARTESIAN_POINT('Ctrl Pts',(0.31375413094027,-0.150066513117541,
-5.5051180226893));
#29138=CARTESIAN_POINT('Ctrl Pts',(0.296141949136947,0.182377517807546,
-5.4892324372648));
#29139=CARTESIAN_POINT('Ctrl Pts',(0.00719424864184242,0.347720945340898,
-5.47334685184028));
#29140=CARTESIAN_POINT('Ctrl Pts',(-0.288345071828068,0.194470390018404,
-5.45746126641578));
#29141=CARTESIAN_POINT('Ctrl Pts',(-0.319692642848795,-0.136960677384898,
-5.44157568099127));
#29142=CARTESIAN_POINT('Ctrl Pts',(-0.0581267332803917,-0.34290362482743,
-5.42569009556676));
#29143=CARTESIAN_POINT('Ctrl Pts',(0.256696904113111,-0.234666385450186,
-5.40980451014226));
#29144=CARTESIAN_POINT('Ctrl Pts',(0.336325940309834,0.0885803303009154,
-5.39391892471776));
#29145=CARTESIAN_POINT('Ctrl Pts',(0.107801492238604,0.330666677052099,
-5.37803333929324));
#29146=CARTESIAN_POINT('Ctrl Pts',(-0.219494419645449,0.269784752693763,
-5.36214775386874));
#29147=CARTESIAN_POINT('Ctrl Pts',(-0.345681936117525,-0.0382833133828322,
-5.34626216844423));
#29148=CARTESIAN_POINT('Ctrl Pts',(-0.155143680664333,-0.311274880758883,
-5.33037658301973));
#29149=CARTESIAN_POINT('Ctrl Pts',(0.177542592615962,-0.299065612949288,
-5.31449099759522));
#29150=CARTESIAN_POINT('Ctrl Pts',(0.34755818854623,-0.0128420643198113,
-5.29860541217071));
#29151=CARTESIAN_POINT('Ctrl Pts',(0.199128925041234,0.28514782877212,-5.28271982674621));
#29152=CARTESIAN_POINT('Ctrl Pts',(-0.13174916180897,0.321875397326613,
-5.26683424132169));
#29153=CARTESIAN_POINT('Ctrl Pts',(-0.341914099910008,0.0636895699801798,
-5.25094865589719));
#29154=CARTESIAN_POINT('Ctrl Pts',(-0.238805488220131,-0.252850848994968,
-5.23506307047268));
#29155=CARTESIAN_POINT('Ctrl Pts',(0.0831049892716063,-0.337720555784953,
-5.21917748504817));
#29156=CARTESIAN_POINT('Ctrl Pts',(0.328871795001037,-0.113158983268353,
-5.20329189962367));
#29157=CARTESIAN_POINT('Ctrl Pts',(0.273314862770547,0.215082772044271,
-5.18740631419916));
#29158=CARTESIAN_POINT('Ctrl Pts',(-0.0326626203915411,0.346258236394009,
-5.17152072877465));
#29159=CARTESIAN_POINT('Ctrl Pts',(-0.308713478596589,0.16017990252939,
-5.15563514335015));
#29160=CARTESIAN_POINT('Ctrl Pts',(-0.301910347060617,-0.17266081020101,
-5.13974955792564));
#29161=CARTESIAN_POINT('Ctrl Pts',(-0.0184864907075617,-0.347303703842689,
-5.12386397250114));
#29162=CARTESIAN_POINT('Ctrl Pts',(0.281875329211953,-0.203734905755456,
-5.10797838707663));
#29163=CARTESIAN_POINT('Ctrl Pts',(0.323973202122692,0.12650287486022,-5.09209280165213));
#29164=CARTESIAN_POINT('Ctrl Pts',(0.0692355976640608,0.340834336676386,
-5.07620721622761));
#29165=CARTESIAN_POINT('Ctrl Pts',(-0.248938061224104,0.242881565203116,
-5.06032163080311));
#29166=CARTESIAN_POINT('Ctrl Pts',(-0.339026039708127,-0.0776077150891233,
-5.0444360453786));
#29167=CARTESIAN_POINT('Ctrl Pts',(-0.118486609264369,-0.326990116771997,
-5.02855045995409));
#29168=CARTESIAN_POINT('Ctrl Pts',(0.210614359579554,-0.276772839311276,
-5.01266487452959));
#29169=CARTESIAN_POINT('Ctrl Pts',(0.346743151845229,0.027033307048315,
-4.99677928910507));
#29170=CARTESIAN_POINT('Ctrl Pts',(0.165173849551959,0.306070600459629,
-4.98089370368058));
#29171=CARTESIAN_POINT('Ctrl Pts',(-0.167733458969751,0.304675400686655,
-4.96500811825607));
#29172=CARTESIAN_POINT('Ctrl Pts',(-0.346957558393056,0.0241260381219176,
-4.94912253283156));
#29173=CARTESIAN_POINT('Ctrl Pts',(-0.208287116546523,-0.278528436828748,
-4.93323694740706));
#29174=CARTESIAN_POINT('Ctrl Pts',(0.121223201144314,-0.325985503582378,
-4.91735136198254));
#29175=CARTESIAN_POINT('Ctrl Pts',(0.33966462009862,-0.074763352618723,
-4.90146577655805));
#29176=CARTESIAN_POINT('Ctrl Pts',(0.24689354063685,0.244959573467403,-4.88558019113352));
#29177=CARTESIAN_POINT('Ctrl Pts',(-0.0720899585996865,0.340242047534732,
-4.86969460570903));
#29178=CARTESIAN_POINT('Ctrl Pts',(-0.325022138979386,0.123782964154184,
-4.85380902028452));
#29179=CARTESIAN_POINT('Ctrl Pts',(-0.280157769683282,-0.206090361559246,
-4.83792343486001));
#29180=CARTESIAN_POINT('Ctrl Pts',(0.0213968590472457,-0.347136554491807,
-4.82203784943551));
#29181=CARTESIAN_POINT('Ctrl Pts',(0.30334694385908,-0.170124203724479,
-4.80615226401099));
#29182=CARTESIAN_POINT('Ctrl Pts',(0.307360044071647,0.16276183935372,-4.7902666785865));
#29183=CARTESIAN_POINT('Ctrl Pts',(0.0297592181678009,0.346519843552389,
-4.77438109316198));
#29184=CARTESIAN_POINT('Ctrl Pts',(-0.27510803493774,0.212784355990346,
-4.75849550773748));
#29185=CARTESIAN_POINT('Ctrl Pts',(-0.327911770617026,-0.1159115340781,
-4.74260992231297));
#29186=CARTESIAN_POINT('Ctrl Pts',(-0.0802713759534626,-0.3384052588895,
-4.72672433688846));
#29187=CARTESIAN_POINT('Ctrl Pts',(0.240916435731397,-0.250840355676695,
-4.71083875146396));
#29188=CARTESIAN_POINT('Ctrl Pts',(0.341368258334745,0.0665531760551926,
-4.69495316603944));
#29189=CARTESIAN_POINT('Ctrl Pts',(0.129046650118439,0.322968381013901,
-4.67906758061495));
#29190=CARTESIAN_POINT('Ctrl Pts',(-0.201511971961497,0.283468760532303,
-4.66318199519044));
#29191=CARTESIAN_POINT('Ctrl Pts',(-0.347438340506522,-0.0157547639654172,
-4.64729640976592));
#29192=CARTESIAN_POINT('Ctrl Pts',(-0.175029658544443,-0.300543227625157,
-4.63141082434143));
#29193=CARTESIAN_POINT('Ctrl Pts',(0.157747263467816,-0.309963568681783,
-4.61552523891691));
#29194=CARTESIAN_POINT('Ctrl Pts',(0.345990674842834,-0.0353845441306157,
-4.59963965349241));
#29195=CARTESIAN_POINT('Ctrl Pts',(0.217225437170922,0.271615026254869,
-4.5837540680679));
#29196=CARTESIAN_POINT('Ctrl Pts',(-0.110569275522142,0.329751494844285,
-4.5678684826434));
#29197=CARTESIAN_POINT('Ctrl Pts',(-0.337056585420913,0.085758213985171,
-4.55198289721889));
#29198=CARTESIAN_POINT('Ctrl Pts',(-0.254720968675225,-0.2368097150851,
-4.53609731179438));
#29199=CARTESIAN_POINT('Ctrl Pts',(0.0609988287289104,-0.342404374877472,
-4.52021172636987));
#29200=CARTESIAN_POINT('Ctrl Pts',(0.32082938490543,-0.134276277959789,
-4.50432614094537));
#29201=CARTESIAN_POINT('Ctrl Pts',(0.286704938018275,0.196880399119539,
-4.48844055552086));
#29202=CARTESIAN_POINT('Ctrl Pts',(-0.0101085108702889,0.347648430241697,
-4.47255497009635));
#29203=CARTESIAN_POINT('Ctrl Pts',(-0.297660191717496,0.179888919359239,
-4.45666938467184));
#29204=CARTESIAN_POINT('Ctrl Pts',(-0.312485287392206,-0.152691054763995,
-4.44078379924734));
#29205=CARTESIAN_POINT('Ctrl Pts',(-0.0410005313686208,-0.345370191923133,
-4.42489821382283));
#29206=CARTESIAN_POINT('Ctrl Pts',(0.268050332658533,-0.221609187993598,
-4.40901262839833));
#29207=CARTESIAN_POINT('Ctrl Pts',(0.331504190722268,0.10519783541074,-4.39312704297382));
#29208=CARTESIAN_POINT('Ctrl Pts',(0.0912224186219852,0.33561895563613,
-4.37724145754931));
#29209=CARTESIAN_POINT('Ctrl Pts',(-0.232640495378394,0.258534355457117,
-4.36135587212481));
#29210=CARTESIAN_POINT('Ctrl Pts',(-0.34335012370998,-0.0554283825298268,
-4.3454702867003));
#29211=CARTESIAN_POINT('Ctrl Pts',(-0.139470467469546,-0.318605715179998,
-4.32958470127579));
#29212=CARTESIAN_POINT('Ctrl Pts',(0.192196865402776,-0.289865448045948,
-4.31369911585128));
#29213=CARTESIAN_POINT('Ctrl Pts',(0.347766768250241,0.00445958992670925,
-4.29781353042678));
#29214=CARTESIAN_POINT('Ctrl Pts',(0.18470070370782,0.294698597029859,-4.28192794500227));
#29215=CARTESIAN_POINT('Ctrl Pts',(-0.147594547681994,0.314924534668353,
-4.26604235957776));
#29216=CARTESIAN_POINT('Ctrl Pts',(-0.34465855855177,0.0466056977047642,
-4.25015677415325));
#29217=CARTESIAN_POINT('Ctrl Pts',(-0.225934451494405,-0.264414894946282,
-4.23427118872876));
#29218=CARTESIAN_POINT('Ctrl Pts',(0.0997986313798216,-0.333169395677702,
-4.21838560330424));
#29219=CARTESIAN_POINT('Ctrl Pts',(0.334092748955866,-0.0966625477454723,
-4.20250001787973));
#29220=CARTESIAN_POINT('Ctrl Pts',(0.262279509589452,0.22840987695598,-4.18661443245523));
#29221=CARTESIAN_POINT('Ctrl Pts',(-0.0498433076157462,0.344205255229274,
-4.17072884703072));
#29222=CARTESIAN_POINT('Ctrl Pts',(-0.316297958710795,0.144627847791949,
-4.15484326160621));
#29223=CARTESIAN_POINT('Ctrl Pts',(-0.29294945649027,-0.187462606894199,
-4.13895767618171));
#29224=CARTESIAN_POINT('Ctrl Pts',(-0.00119050799645002,-0.347793323300234,
-4.1230720907572));
#29225=CARTESIAN_POINT('Ctrl Pts',(0.291659225189475,-0.189463741659231,
-4.1071865053327));
#29226=CARTESIAN_POINT('Ctrl Pts',(0.317280666741316,0.142459087297245,
-4.09130091990818));
#29227=CARTESIAN_POINT('Ctrl Pts',(0.0521985638184197,0.343855962543531,
-4.07541533448368));
#29228=CARTESIAN_POINT('Ctrl Pts',(-0.26070967258762,0.230200086145824,
-4.05952974905918));
#29229=CARTESIAN_POINT('Ctrl Pts',(-0.334746670225899,-0.0943730883935936,
-4.04364416363466));
#29230=CARTESIAN_POINT('Ctrl Pts',(-0.102077165595292,-0.332478368176598,
-4.02775857821017));
#29231=CARTESIAN_POINT('Ctrl Pts',(0.224118976374829,-0.265955442650332,
-4.01187299278565));
#29232=CARTESIAN_POINT('Ctrl Pts',(0.344969543732986,0.0442450780110779,
-3.99598740736115));
#29233=CARTESIAN_POINT('Ctrl Pts',(0.149747057815299,0.313906724552109,
-3.98010182193664));
#29234=CARTESIAN_POINT('Ctrl Pts',(-0.182678873120845,0.295956149438136,
-3.96421623651213));
#29235=CARTESIAN_POINT('Ctrl Pts',(-0.347728088273613,0.00684029167798261,
-3.94833065108763));
#29236=CARTESIAN_POINT('Ctrl Pts',(-0.19417677635953,-0.288542878270008,
-3.93244506566312));
#29237=CARTESIAN_POINT('Ctrl Pts',(0.137286029375129,-0.319553061933777,
-3.91655948023861));
#29238=CARTESIAN_POINT('Ctrl Pts',(0.342962614929039,-0.0577776533342563,
-3.9006738948141));
#29239=CARTESIAN_POINT('Ctrl Pts',(0.234404967686561,0.256935642887977,
-3.8847883093896));
#29240=CARTESIAN_POINT('Ctrl Pts',(-0.0889226413224721,0.33623559921306,
-3.86890272396509));
#29241=CARTESIAN_POINT('Ctrl Pts',(-0.330776233655315,0.107464840971431,
-3.85301713854058));
#29242=CARTESIAN_POINT('Ctrl Pts',(-0.26956119552286,-0.219768921902748,
-3.83713155311608));
#29243=CARTESIAN_POINT('Ctrl Pts',(0.0386351925404547,-0.345642795608912,
-3.82124596769157));
#29244=CARTESIAN_POINT('Ctrl Pts',(0.311432602570261,-0.154826730819173,
-3.80536038226707));
#29245=CARTESIAN_POINT('Ctrl Pts',(0.298884813042677,0.177846896358873,
-3.78947479684255));
#29246=CARTESIAN_POINT('Ctrl Pts',(0.0124881160261418,0.347571138851938,
-3.77358921141805));
#29247=CARTESIAN_POINT('Ctrl Pts',(-0.285350081128901,0.198838450950602,
-3.75770362599354));
#29248=CARTESIAN_POINT('Ctrl Pts',(-0.321741695679867,-0.132076520830608,
-3.74181804056904));
#29249=CARTESIAN_POINT('Ctrl Pts',(-0.0633403822416737,-0.341979173492766,
-3.72593245514453));
#29250=CARTESIAN_POINT('Ctrl Pts',(0.253091653661904,-0.238547170777931,
-3.71004686972002));
#29251=CARTESIAN_POINT('Ctrl Pts',(0.337639941368927,0.0834471524521679,
-3.69416128429552));
#29252=CARTESIAN_POINT('Ctrl Pts',(0.112816128339058,0.32898984082218,-3.678275698871));
#29253=CARTESIAN_POINT('Ctrl Pts',(-0.215345354819328,0.2730899292435,-3.66239011344651));
#29254=CARTESIAN_POINT('Ctrl Pts',(-0.346254804611121,-0.0330037517386558,
-3.64650452802199));
#29255=CARTESIAN_POINT('Ctrl Pts',(-0.159807574965718,-0.308898259594252,
-3.63061894259749));
#29256=CARTESIAN_POINT('Ctrl Pts',(0.172855681678712,-0.301691929331577,
-3.61473335717298));
#29257=CARTESIAN_POINT('Ctrl Pts',(0.347542139351973,-0.0182170469437311,
-3.59884777174848));
#29258=CARTESIAN_POINT('Ctrl Pts',(0.202997430525575,0.282263936041357,
-3.58296218632397));
#29259=CARTESIAN_POINT('Ctrl Pts',(-0.0161459929656535,0.309635118478954,
-3.57237179604096));
#29260=CARTESIAN_POINT('Ctrl Pts',(-0.107287652231604,0.273939773816491,
-3.56707660089946));
#29261=CARTESIAN_POINT('',(0.29192076924273,-0.0365500271509186,-3.6));
#29262=CARTESIAN_POINT('Ctrl Pts',(0.292414323780515,-0.0364994916172054,
-3.6));
#29263=CARTESIAN_POINT('Ctrl Pts',(0.292666487654641,-0.0294203594636345,
-3.6));
#29264=CARTESIAN_POINT('Ctrl Pts',(0.292644719912668,-0.0223426691634168,
-3.6));
#29265=CARTESIAN_POINT('Ctrl Pts',(0.292340298090172,-0.0152783476836462,
-3.6));
#29266=CARTESIAN_POINT('Ctrl Pts',(0.291819266745405,-0.00318745061757684,
-3.6));
#29267=CARTESIAN_POINT('Ctrl Pts',(0.290470817834819,0.0088645857384901,
-3.6));
#29268=CARTESIAN_POINT('Ctrl Pts',(0.288335912431399,0.020809913429241,
-3.6));
#29269=CARTESIAN_POINT('Ctrl Pts',(0.287324186550805,0.0264707718249139,
-3.6));
#29270=CARTESIAN_POINT('Ctrl Pts',(0.286135672242458,0.0321076021086892,
-3.6));
#29271=CARTESIAN_POINT('Ctrl Pts',(0.284773910663568,0.0377127213804415,
-3.6));
#29272=CARTESIAN_POINT('Ctrl Pts',(0.283356850440654,0.0435454542815746,
-3.6));
#29273=CARTESIAN_POINT('Ctrl Pts',(0.281753731857198,0.0493368411209126,
-3.6));
#29274=CARTESIAN_POINT('Ctrl Pts',(0.279972018733966,0.055071055872317,
-3.6));
#29275=CARTESIAN_POINT('Ctrl Pts',(0.274848939028037,0.0715590296315548,
-3.6));
#29276=CARTESIAN_POINT('Ctrl Pts',(0.268247408855639,0.0875967881401878,
-3.6));
#29277=CARTESIAN_POINT('Ctrl Pts',(0.260271123750079,0.102974430970234,
-3.6));
#29278=CARTESIAN_POINT('Ctrl Pts',(0.257522628682807,0.108273310699995,
-3.6));
#29279=CARTESIAN_POINT('Ctrl Pts',(0.254608896221931,0.113495680260488,
-3.6));
#29280=CARTESIAN_POINT('Ctrl Pts',(0.251546120022716,0.118612125015772,
-3.6));
#29281=CARTESIAN_POINT('Ctrl Pts',(0.242945994386678,0.132978851424501,
-3.6));
#29282=CARTESIAN_POINT('Ctrl Pts',(0.233156507997209,0.146548580458849,
-3.6));
#29283=CARTESIAN_POINT('Ctrl Pts',(0.222274509229499,0.159129353049593,
-3.6));
#29284=CARTESIAN_POINT('Ctrl Pts',(0.215201410731259,0.167306623201684,
-3.6));
#29285=CARTESIAN_POINT('Ctrl Pts',(0.207665946000832,0.175065453049953,
-3.6));
#29286=CARTESIAN_POINT('Ctrl Pts',(0.199688444759937,0.182342711212395,
-3.6));
#29287=CARTESIAN_POINT('Ctrl Pts',(0.196404264508349,0.185338615170426,
-3.6));
#29288=CARTESIAN_POINT('Ctrl Pts',(0.193045123181327,0.188252788830684,
-3.6));
#29289=CARTESIAN_POINT('Ctrl Pts',(0.189612281823844,0.191080315392676,
-3.6));
#29290=CARTESIAN_POINT('Ctrl Pts',(0.186193494325361,0.193896266220318,
-3.6));
#29291=CARTESIAN_POINT('Ctrl Pts',(0.182708690605058,0.19662039211184,-3.6));
#29292=CARTESIAN_POINT('Ctrl Pts',(0.179161622624937,0.199247529650452,
-3.6));
#29293=CARTESIAN_POINT('Ctrl Pts',(0.171408656339104,0.204989767712777,
-3.6));
#29294=CARTESIAN_POINT('Ctrl Pts',(0.163355483608744,0.210271516086989,
-3.6));
#29295=CARTESIAN_POINT('Ctrl Pts',(0.155019203531841,0.215050497759424,
-3.6));
#29296=CARTESIAN_POINT('Ctrl Pts',(0.140808457822457,0.223197164218598,
-3.6));
#29297=CARTESIAN_POINT('Ctrl Pts',(0.125774643211521,0.22988578386622,-3.6));
#29298=CARTESIAN_POINT('Ctrl Pts',(0.11014676513074,0.235093491948397,-3.6));
#29299=CARTESIAN_POINT('Ctrl Pts',(0.106087966374167,0.236446013319454,
-3.6));
#29300=CARTESIAN_POINT('Ctrl Pts',(0.101986598043523,0.237699037569938,
-3.6));
#29301=CARTESIAN_POINT('Ctrl Pts',(0.0978550841807309,0.23884928488335,
-3.6));
#29302=CARTESIAN_POINT('Ctrl Pts',(0.0826054374270896,0.243094911496596,
-3.6));
#29303=CARTESIAN_POINT('Ctrl Pts',(0.0670045393815982,0.245930050485186,
-3.6));
#29304=CARTESIAN_POINT('Ctrl Pts',(0.051262317664912,0.247351840499526,
-3.6));
#29305=CARTESIAN_POINT('Ctrl Pts',(0.039125047109517,0.248448042191229,
-3.6));
#29306=CARTESIAN_POINT('Ctrl Pts',(0.026903246465002,0.248702971880079,
-3.6));
#29307=CARTESIAN_POINT('Ctrl Pts',(0.0146976872519464,0.248094407813563,
-3.6));
#29308=CARTESIAN_POINT('Ctrl Pts',(0.0102876623740829,0.247874525821574,
-3.6));
#29309=CARTESIAN_POINT('Ctrl Pts',(0.00587781616497291,0.247541537797545,
-3.6));
#29310=CARTESIAN_POINT('Ctrl Pts',(0.00147967530992972,0.247094507554182,
-3.6));
#29311=CARTESIAN_POINT('Ctrl Pts',(-0.0139171193363565,0.245529566119927,
-3.6));
#29312=CARTESIAN_POINT('Ctrl Pts',(-0.0290846126574327,0.242581300092628,
-3.6));
#29313=CARTESIAN_POINT('Ctrl Pts',(-0.0438193177938728,0.238223133415296,
-3.6));
#29314=CARTESIAN_POINT('Ctrl Pts',(-0.0576495230985568,0.234132495744477,
-3.6));
#29315=CARTESIAN_POINT('Ctrl Pts',(-0.0710995093010162,0.228799086735258,
-3.6));
#29316=CARTESIAN_POINT('Ctrl Pts',(-0.0839735920665051,0.222161024970596,
-3.6));
#29317=CARTESIAN_POINT('Ctrl Pts',(-0.084815561179679,0.221726893617008,
-3.6));
#29318=CARTESIAN_POINT('Ctrl Pts',(-0.0856550535821104,0.221287168938323,
-3.6));
#29319=CARTESIAN_POINT('Ctrl Pts',(-0.0864920085589077,0.220841828194855,
-3.6));
#29320=CARTESIAN_POINT('Ctrl Pts',(-0.294584692827634,-0.000157098441292656,
-3.64801761170896));
#29321=CARTESIAN_POINT('Ctrl Pts',(-0.294645466431812,-0.00944699213001965,
-3.64751325047997));
#29322=CARTESIAN_POINT('Ctrl Pts',(-0.294243676282554,-0.0187316056112418,
-3.64700888925098));
#29323=CARTESIAN_POINT('Ctrl Pts',(-0.293362024704922,-0.0279705562175625,
-3.64650452802199));
#29324=CARTESIAN_POINT('Ctrl Pts',(-0.284105728062653,-0.124968587690521,
-3.64120933288049));
#29325=CARTESIAN_POINT('Ctrl Pts',(-0.221956651514186,-0.216933423642387,
-3.63591413773899));
#29326=CARTESIAN_POINT('Ctrl Pts',(-0.135438237132546,-0.26171478657454,
-3.63061894259749));
#29327=CARTESIAN_POINT('Ctrl Pts',(-0.048919822750907,-0.306496149506694,
-3.62532374745599));
#29328=CARTESIAN_POINT('Ctrl Pts',(0.0619679294639041,-0.304094039419135,
-3.62002855231448));
#29329=CARTESIAN_POINT('Ctrl Pts',(0.14652621518352,-0.255647170644047,
-3.61473335717298));
#29330=CARTESIAN_POINT('Ctrl Pts',(0.224951239641238,-0.210714295808048,
-3.60982223811532));
#29331=CARTESIAN_POINT('Ctrl Pts',(0.280727784900505,-0.126173943185802,
-3.60491111905766));
#29332=CARTESIAN_POINT('Ctrl Pts',(0.292414323780514,-0.0364994916172137,
-3.6));
#29333=CARTESIAN_POINT('',(-0.137702479013098,-0.193106208855768,-5.9658));
#29334=CARTESIAN_POINT('Ctrl Pts',(-0.138001922973978,-0.193371366051279,
-5.9658));
#29335=CARTESIAN_POINT('Ctrl Pts',(-0.143073358296614,-0.190612953673137,
-5.9658));
#29336=CARTESIAN_POINT('Ctrl Pts',(-0.148027594123821,-0.187662423150088,
-5.9658));
#29337=CARTESIAN_POINT('Ctrl Pts',(-0.152852356931864,-0.184522195146066,
-5.9658));
#29338=CARTESIAN_POINT('Ctrl Pts',(-0.162997379060741,-0.177919242035622,
-5.9658));
#29339=CARTESIAN_POINT('Ctrl Pts',(-0.172570666260329,-0.17047916665888,
-5.9658));
#29340=CARTESIAN_POINT('Ctrl Pts',(-0.181542838702178,-0.162315875140337,
-5.9658));
#29341=CARTESIAN_POINT('Ctrl Pts',(-0.186610812592755,-0.15770480145163,
-5.9658));
#29342=CARTESIAN_POINT('Ctrl Pts',(-0.191489654388371,-0.152858842458079,
-5.9658));
#29343=CARTESIAN_POINT('Ctrl Pts',(-0.19615336760798,-0.147818230112143,
-5.9658));
#29344=CARTESIAN_POINT('Ctrl Pts',(-0.203092451016376,-0.140318362978212,
-5.9658));
#29345=CARTESIAN_POINT('Ctrl Pts',(-0.209564344127366,-0.132381113357134,
-5.9658));
#29346=CARTESIAN_POINT('Ctrl Pts',(-0.215551335673081,-0.124070288249604,
-5.9658));
#29347=CARTESIAN_POINT('Ctrl Pts',(-0.219342144904121,-0.118808087310347,
-5.9658));
#29348=CARTESIAN_POINT('Ctrl Pts',(-0.222938463172683,-0.113395908629678,
-5.9658));
#29349=CARTESIAN_POINT('Ctrl Pts',(-0.226334587133058,-0.107848190686934,
-5.9658));
#29350=CARTESIAN_POINT('Ctrl Pts',(-0.228858498148498,-0.103725270973279,
-5.9658));
#29351=CARTESIAN_POINT('Ctrl Pts',(-0.231271645540891,-0.0995272197569029,
-5.9658));
#29352=CARTESIAN_POINT('Ctrl Pts',(-0.233564764998697,-0.0952733717887619,
-5.9658));
#29353=CARTESIAN_POINT('Ctrl Pts',(-0.241164174912553,-0.0811760973048323,
-5.9658));
#29354=CARTESIAN_POINT('Ctrl Pts',(-0.247469655098504,-0.0664351633284274,
-5.9658));
#29355=CARTESIAN_POINT('Ctrl Pts',(-0.252411117523312,-0.051269455660209,
-5.9658));
#29356=CARTESIAN_POINT('Ctrl Pts',(-0.255809694565027,-0.0408389754760835,
-5.9658));
#29357=CARTESIAN_POINT('Ctrl Pts',(-0.258562495027418,-0.0302064884413545,
-5.9658));
#29358=CARTESIAN_POINT('Ctrl Pts',(-0.260635400953148,-0.0194347400518625,
-5.9658));
#29359=CARTESIAN_POINT('Ctrl Pts',(-0.261801443193027,-0.0133754618841457,
-5.9658));
#29360=CARTESIAN_POINT('Ctrl Pts',(-0.262752444669097,-0.00726639468052522,
-5.9658));
#29361=CARTESIAN_POINT('Ctrl Pts',(-0.263478002042444,-0.00115090105513363,
-5.9658));
#29362=CARTESIAN_POINT('Ctrl Pts',(-0.264780382498361,0.0098264518993917,
-5.9658));
#29363=CARTESIAN_POINT('Ctrl Pts',(-0.265361291178618,0.0208402687922307,
-5.9658));
#29364=CARTESIAN_POINT('Ctrl Pts',(-0.265195455964071,0.0318245246133395,
-5.9658));
#29365=CARTESIAN_POINT('Ctrl Pts',(-0.26502005174603,0.0434425926354643,
-5.9658));
#29366=CARTESIAN_POINT('Ctrl Pts',(-0.26400964329553,0.0550278502294863,
-5.9658));
#29367=CARTESIAN_POINT('Ctrl Pts',(-0.262217575180139,0.0665215726485518,
-5.9658));
#29368=CARTESIAN_POINT('Ctrl Pts',(-0.261084137053752,0.0737910637421093,
-5.9658));
#29369=CARTESIAN_POINT('Ctrl Pts',(-0.259637700833268,0.0810240070529162,
-5.9658));
#29370=CARTESIAN_POINT('Ctrl Pts',(-0.257888733163235,0.0882056483398937,
-5.9658));
#29371=CARTESIAN_POINT('Ctrl Pts',(-0.256841146357813,0.0925072673934748,
-5.9658));
#29372=CARTESIAN_POINT('Ctrl Pts',(-0.2556849101705,0.0967898034443975,
-5.9658));
#29373=CARTESIAN_POINT('Ctrl Pts',(-0.254426565527262,0.10103697054799,
-5.9658));
#29374=CARTESIAN_POINT('Ctrl Pts',(-0.249729836042933,0.116889380352809,
-5.9658));
#29375=CARTESIAN_POINT('Ctrl Pts',(-0.243603775465189,0.132296506950611,
-5.9658));
#29376=CARTESIAN_POINT('Ctrl Pts',(-0.236195443982762,0.147098364696853,
-5.9658));
#29377=CARTESIAN_POINT('Ctrl Pts',(-0.229442030401605,0.160591695464646,
-5.9658));
#29378=CARTESIAN_POINT('Ctrl Pts',(-0.221622050217669,0.173582952148739,
-5.9658));
#29379=CARTESIAN_POINT('Ctrl Pts',(-0.212811980334952,0.185945226493148,
-5.9658));
#29380=CARTESIAN_POINT('Ctrl Pts',(-0.210205025895605,0.189603300312268,
-5.9658));
#29381=CARTESIAN_POINT('Ctrl Pts',(-0.207511908992761,0.193204856844324,
-5.9658));
#29382=CARTESIAN_POINT('Ctrl Pts',(-0.204742504452648,0.196736924240536,
-5.9658));
#29383=CARTESIAN_POINT('Ctrl Pts',(-0.193966565401581,0.210480435682992,
-5.9658));
#29384=CARTESIAN_POINT('Ctrl Pts',(-0.182010459766652,0.223214646370377,
-5.9658));
#29385=CARTESIAN_POINT('Ctrl Pts',(-0.169008886945702,0.234760544715186,
-5.9658));
#29386=CARTESIAN_POINT('Ctrl Pts',(-0.156567866754381,0.245808650695352,
-5.9658));
#29387=CARTESIAN_POINT('Ctrl Pts',(-0.143168667892983,0.255769903558261,
-5.9658));
#29388=CARTESIAN_POINT('Ctrl Pts',(-0.128892185405323,0.264462557919717,
-5.9658));
#29389=CARTESIAN_POINT('Ctrl Pts',(-0.138001922973973,-0.193371366051283,
-5.9658));
#29390=CARTESIAN_POINT('Ctrl Pts',(-0.0784315765852419,-0.235399718049311,
-5.96088888094234));
#29391=CARTESIAN_POINT('Ctrl Pts',(0.0890659557212074,-0.262569296818482,
-5.95068256674318));
#29392=CARTESIAN_POINT('Ctrl Pts',(0.270472008799548,-0.0738624404218237,
-5.93518105740252));
#29393=CARTESIAN_POINT('Ctrl Pts',(0.208622919271946,0.187359333710957,
-5.91929547197799));
#29394=CARTESIAN_POINT('Ctrl Pts',(-0.0444078770673998,0.276831260195588,
-5.90340988655351));
#29395=CARTESIAN_POINT('Ctrl Pts',(-0.215288460980913,0.144741092199657,
-5.89062506616399));
#29396=CARTESIAN_POINT('Ctrl Pts',(-0.236965055372185,0.0329209448004622,
-5.88313544091599));
#29397=CARTESIAN_POINT('Ctrl Pts',(-0.23683200269258,0.000108453577955931,
-5.8809410108095));
#29398=CARTESIAN_POINT('Origin',(-3.51939854619125E-17,0.,-5.9658));
#29399=CARTESIAN_POINT('',(-0.2942,-3.60291088309151E-17,-5.9658));
#29400=CARTESIAN_POINT('Origin',(0.,0.,-5.9658));
#29401=CARTESIAN_POINT('Origin',(0.,0.,-5.9658));
#29402=CARTESIAN_POINT('',(0.137702479013101,-0.193106208855765,-5.9658));
#29403=CARTESIAN_POINT('Ctrl Pts',(0.129204211840496,0.264848286765706,
-5.9658));
#29404=CARTESIAN_POINT('Ctrl Pts',(0.135270963946878,0.261191483925809,
-5.9658));
#29405=CARTESIAN_POINT('Ctrl Pts',(0.141186833539423,0.257306043876668,
-5.9658));
#29406=CARTESIAN_POINT('Ctrl Pts',(0.14693706551556,0.253191178187327,-5.9658));
#29407=CARTESIAN_POINT('Ctrl Pts',(0.156778842106654,0.246148403394085,
-5.9658));
#29408=CARTESIAN_POINT('Ctrl Pts',(0.166135974562664,0.23843387751087,-5.9658));
#29409=CARTESIAN_POINT('Ctrl Pts',(0.174974019412259,0.230118978005656,
-5.9658));
#29410=CARTESIAN_POINT('Ctrl Pts',(0.179162346603656,0.22617856807517,-5.9658));
#29411=CARTESIAN_POINT('Ctrl Pts',(0.183233953121907,0.22210322175818,-5.9658));
#29412=CARTESIAN_POINT('Ctrl Pts',(0.187184339205463,0.217900102741158,
-5.9658));
#29413=CARTESIAN_POINT('Ctrl Pts',(0.191295138666803,0.213526307616919,
-5.9658));
#29414=CARTESIAN_POINT('Ctrl Pts',(0.195269648419525,0.20901927500812,-5.9658));
#29415=CARTESIAN_POINT('Ctrl Pts',(0.199098691984892,0.204393903223475,
-5.9658));
#29416=CARTESIAN_POINT('Ctrl Pts',(0.210108605301767,0.191094252399997,
-5.9658));
#29417=CARTESIAN_POINT('Ctrl Pts',(0.219933632950231,0.176802353940203,
-5.9658));
#29418=CARTESIAN_POINT('Ctrl Pts',(0.228454636692493,0.1617197431557,-5.9658));
#29419=CARTESIAN_POINT('Ctrl Pts',(0.231390832132516,0.156522527622341,
-5.9658));
#29420=CARTESIAN_POINT('Ctrl Pts',(0.234172663418191,0.151228725911185,
-5.9658));
#29421=CARTESIAN_POINT('Ctrl Pts',(0.236784343132879,0.145867972582067,
-5.9658));
#29422=CARTESIAN_POINT('Ctrl Pts',(0.244117814256368,0.130815234867661,
-5.9658));
#29423=CARTESIAN_POINT('Ctrl Pts',(0.250133917516935,0.115201848504892,
-5.9658));
#29424=CARTESIAN_POINT('Ctrl Pts',(0.254724799740319,0.0992138111912858,
-5.9658));
#29425=CARTESIAN_POINT('Ctrl Pts',(0.257708789856447,0.0888218771361952,
-5.9658));
#29426=CARTESIAN_POINT('Ctrl Pts',(0.260089689774926,0.0782713310743704,
-5.9658));
#29427=CARTESIAN_POINT('Ctrl Pts',(0.261825733325987,0.0676136941592587,
-5.9658));
#29428=CARTESIAN_POINT('Ctrl Pts',(0.262540428182012,0.0632261554503647,
-5.9658));
#29429=CARTESIAN_POINT('Ctrl Pts',(0.263145713290975,0.0588204915595365,
-5.9658));
#29430=CARTESIAN_POINT('Ctrl Pts',(0.263638159729527,0.0544004451437594,
-5.9658));
#29431=CARTESIAN_POINT('Ctrl Pts',(0.264128588802814,0.0499985059725725,
-5.9658));
#29432=CARTESIAN_POINT('Ctrl Pts',(0.26450604161011,0.0455914489729751,
-5.9658));
#29433=CARTESIAN_POINT('Ctrl Pts',(0.264768243741406,0.0411852375561797,
-5.9658));
#29434=CARTESIAN_POINT('Ctrl Pts',(0.265341350360721,0.031554389337699,
-5.9658));
#29435=CARTESIAN_POINT('Ctrl Pts',(0.265364753733676,0.0219237178920483,
-5.9658));
#29436=CARTESIAN_POINT('Ctrl Pts',(0.26481238867451,0.0123306438726335,
-5.9658));
#29437=CARTESIAN_POINT('Ctrl Pts',(0.263870782204104,-0.00402249146400645,
-5.9658));
#29438=CARTESIAN_POINT('Ctrl Pts',(0.261258313698482,-0.020268305434637,
-5.9658));
#29439=CARTESIAN_POINT('Ctrl Pts',(0.257080958864981,-0.0362025073647849,
-5.9658));
#29440=CARTESIAN_POINT('Ctrl Pts',(0.255996044923037,-0.0403408289861939,
-5.9658));
#29441=CARTESIAN_POINT('Ctrl Pts',(0.254804542204504,-0.0444604395475238,
-5.9658));
#29442=CARTESIAN_POINT('Ctrl Pts',(0.253510491762343,-0.0485491427174342,
-5.9658));
#29443=CARTESIAN_POINT('Ctrl Pts',(0.248734016185539,-0.0636409739131856,
-5.9658));
#29444=CARTESIAN_POINT('Ctrl Pts',(0.242584291373476,-0.078256306454302,
-5.9658));
#29445=CARTESIAN_POINT('Ctrl Pts',(0.235173624314207,-0.0922177548230339,
-5.9658));
#29446=CARTESIAN_POINT('Ctrl Pts',(0.229460014360973,-0.10298200448142,
-5.9658));
#29447=CARTESIAN_POINT('Ctrl Pts',(0.222995632074016,-0.113357386780667,
-5.9658));
#29448=CARTESIAN_POINT('Ctrl Pts',(0.215816926629553,-0.123247361184162,
-5.9658));
#29449=CARTESIAN_POINT('Ctrl Pts',(0.213223159570887,-0.126820747781132,
-5.9658));
#29450=CARTESIAN_POINT('Ctrl Pts',(0.210534760635697,-0.130332183901753,
-5.9658));
#29451=CARTESIAN_POINT('Ctrl Pts',(0.207757243033476,-0.133771505040915,
-5.9658));
#29452=CARTESIAN_POINT('Ctrl Pts',(0.198033824944794,-0.145811737423448,
-5.9658));
#29453=CARTESIAN_POINT('Ctrl Pts',(0.187277114682385,-0.156904076768832,
-5.9658));
#29454=CARTESIAN_POINT('Ctrl Pts',(0.175576038540493,-0.166863573434083,
-5.9658));
#29455=CARTESIAN_POINT('Ctrl Pts',(0.164593283736169,-0.176211663175789,
-5.9658));
#29456=CARTESIAN_POINT('Ctrl Pts',(0.152777422469776,-0.18456226563307,
-5.9658));
#29457=CARTESIAN_POINT('Ctrl Pts',(0.140183547508633,-0.191717677594505,
-5.9658));
#29458=CARTESIAN_POINT('Ctrl Pts',(0.139359851699299,-0.19218567357389,
-5.9658));
#29459=CARTESIAN_POINT('Ctrl Pts',(0.138532824156898,-0.192648538423476,
-5.9658));
#29460=CARTESIAN_POINT('Ctrl Pts',(0.137702479013101,-0.193106208855765,
-5.9658));
#29461=CARTESIAN_POINT('Origin',(0.,0.,-5.9658));
#29462=CARTESIAN_POINT('Origin',(0.,0.,-6.1506589891905));
#29463=CARTESIAN_POINT('Ctrl Pts',(0.137702479013101,-0.193106208855765,
-5.9658));
#29464=CARTESIAN_POINT('Ctrl Pts',(0.201950251596361,-0.147291640757684,
-5.9605048048585));
#29465=CARTESIAN_POINT('Ctrl Pts',(0.279999109649734,0.0127284642187734,
-5.9499144145755));
#29466=CARTESIAN_POINT('Ctrl Pts',(0.140787666388597,0.242681034292982,
-5.93402882915098));
#29467=CARTESIAN_POINT('Ctrl Pts',(-0.127558649843965,0.249601560230261,
-5.91814324372648));
#29468=CARTESIAN_POINT('Ctrl Pts',(-0.233570227134833,0.0945490249099159,
-5.90701996373965));
#29469=CARTESIAN_POINT('Ctrl Pts',(-0.237519260455749,0.00806361963123399,
-5.90119187889433));
#29470=CARTESIAN_POINT('Ctrl Pts',(-0.237465179907043,0.000150546841787677,
-5.9006589891905));
#29471=CARTESIAN_POINT('Ctrl Pts',(0.170810875200398,-0.239535560853235,
-5.99872339910054));
#29472=CARTESIAN_POINT('Ctrl Pts',(0.250506014629069,-0.182705600130328,
-5.99342820395904));
#29473=CARTESIAN_POINT('Ctrl Pts',(0.347320493555188,0.0157888233294544,
-5.98283781367603));
#29474=CARTESIAN_POINT('Ctrl Pts',(0.174637847376516,0.301029873675537,
-5.96695222825153));
#29475=CARTESIAN_POINT('Ctrl Pts',(-0.158228121783892,0.309614331273291,
-5.95106664282702));
#29476=CARTESIAN_POINT('Ctrl Pts',(-0.346028909939958,0.0349368943093817,
-5.93518105740251));
#29477=CARTESIAN_POINT('Ctrl Pts',(-0.216833251566021,-0.271965029219739,
-5.919295471978));
#29478=CARTESIAN_POINT('Ctrl Pts',(0.111056996638582,-0.329572597154436,
-5.9034098865535));
#29479=CARTESIAN_POINT('Ctrl Pts',(0.337180324851565,-0.0852715125928928,
-5.88752430112899));
#29480=CARTESIAN_POINT('Ctrl Pts',(0.25437389699959,0.237187870968243,-5.87163871570449));
#29481=CARTESIAN_POINT('Ctrl Pts',(-0.0615020985666884,0.342312200380475,
-5.85575313027997));
#29482=CARTESIAN_POINT('Ctrl Pts',(-0.321025987744245,0.133806145032197,
-5.83986754485548));
#29483=CARTESIAN_POINT('Ctrl Pts',(-0.286415645896083,-0.197301835163802,
-5.82398195943096));
#29484=CARTESIAN_POINT('Ctrl Pts',(0.0106191074128067,-0.347632915551424,
-5.80809637400646));
#29485=CARTESIAN_POINT('Ctrl Pts',(0.297924023820578,-0.179451765614445,
-5.79221078858195));
#29486=CARTESIAN_POINT('Ctrl Pts',(0.312260748456384,0.153149879487187,
-5.77632520315744));
#29487=CARTESIAN_POINT('Ctrl Pts',(0.0404932868106416,0.345430002986954,
-5.76043961773294));
#29488=CARTESIAN_POINT('Ctrl Pts',(-0.26837549419498,0.221215336287527,
-5.74455403230843));
#29489=CARTESIAN_POINT('Ctrl Pts',(-0.331349362349014,-0.105684567869114,
-5.72866844688393));
#29490=CARTESIAN_POINT('Ctrl Pts',(-0.0907294504682248,-0.335752567049075,
-5.71278286145941));
#29491=CARTESIAN_POINT('Ctrl Pts',(0.233019924150162,-0.258192447446947,
-5.69689727603491));
#29492=CARTESIAN_POINT('Ctrl Pts',(0.343268369714444,0.0559325528732654,
-5.6810116906104));
#29493=CARTESIAN_POINT('Ctrl Pts',(0.139002435305783,0.318810203883323,
-5.66512610518591));
#29494=CARTESIAN_POINT('Ctrl Pts',(-0.192622347799029,0.289582898383506,
-5.64924051976138));
#29495=CARTESIAN_POINT('Ctrl Pts',(-0.347759859492789,-0.00497029766718102,
-5.63335493433689));
#29496=CARTESIAN_POINT('Ctrl Pts',(-0.184267733667245,-0.294969533934804,
-5.61746934891237));
#29497=CARTESIAN_POINT('Ctrl Pts',(0.148056876757647,-0.314707459357535,
-5.60158376348787));
#29498=CARTESIAN_POINT('Ctrl Pts',(0.344726644784264,-0.0460995018935765,
-5.58569817806336));
#29499=CARTESIAN_POINT('Ctrl Pts',(0.225545911893637,0.264746417001876,
-5.56981259263886));
#29500=CARTESIAN_POINT('Ctrl Pts',(-0.100287803351684,0.333022492034977,
-5.55392700721435));
#29501=CARTESIAN_POINT('Ctrl Pts',(-0.334234356988874,0.0961718165849793,
-5.53804142178984));
#29502=CARTESIAN_POINT('Ctrl Pts',(-0.261943807492036,-0.228794810720281,
-5.52215583636533));
#29503=CARTESIAN_POINT('Ctrl Pts',(0.0503487379441082,-0.344131701947668,
-5.50627025094083));
#29504=CARTESIAN_POINT('Ctrl Pts',(0.31651002448484,-0.144163199526538,
-5.49038466551631));
#29505=CARTESIAN_POINT('Ctrl Pts',(0.292673855696793,0.187892623294873,
-5.47449908009182));
#29506=CARTESIAN_POINT('Ctrl Pts',(0.000679755635424282,0.347794711905736,
-5.4586134946673));
#29507=CARTESIAN_POINT('Ctrl Pts',(-0.291937160100985,0.18903523018041,
-5.4427279092428));
#29508=CARTESIAN_POINT('Ctrl Pts',(-0.317071130604053,-0.142924881789908,
-5.42684232381829));
#29509=CARTESIAN_POINT('Ctrl Pts',(-0.0516935409033043,-0.343932262990989,
-5.41095673839378));
#29510=CARTESIAN_POINT('Ctrl Pts',(0.26104746277864,-0.229816983432556,
-5.39507115296928));
#29511=CARTESIAN_POINT('Ctrl Pts',(0.334607732615142,0.0948645822810613,
-5.37918556754477));
#29512=CARTESIAN_POINT('Ctrl Pts',(0.101588799630167,0.332627929505195,
-5.36329998212027));
#29513=CARTESIAN_POINT('Ctrl Pts',(-0.224509312854917,0.26562603814126,
-5.34741439669575));
#29514=CARTESIAN_POINT('Ctrl Pts',(-0.3449042109429,-0.0447516365182755,
-5.33152881127126));
#29515=CARTESIAN_POINT('Ctrl Pts',(-0.14928591586817,-0.314126310615031,
-5.31564322584674));
#29516=CARTESIAN_POINT('Ctrl Pts',(0.18311330988511,-0.295687570655462,
-5.29975764042224));
#29517=CARTESIAN_POINT('Ctrl Pts',(0.347737774033734,-0.00632962931557787,
-5.28387205499772));
#29518=CARTESIAN_POINT('Ctrl Pts',(0.193752836298635,0.288827737801347,
-5.26798646957323));
#29519=CARTESIAN_POINT('Ctrl Pts',(-0.137755165929293,0.319351120174961,
-5.25210088414871));
#29520=CARTESIAN_POINT('Ctrl Pts',(-0.343047110252429,0.057273936870683,
-5.23621529872421));
#29521=CARTESIAN_POINT('Ctrl Pts',(-0.23402740143643,-0.257279612628208,
-5.2203297132997));
#29522=CARTESIAN_POINT('Ctrl Pts',(0.0894163244517817,-0.336104663191011,
-5.2044441278752));
#29523=CARTESIAN_POINT('Ctrl Pts',(0.330933714521616,-0.106978971251994,
-5.18855854245068));
#29524=CARTESIAN_POINT('Ctrl Pts',(0.269238164496358,0.220164562261598,
-5.17267295702619));
#29525=CARTESIAN_POINT('Ctrl Pts',(-0.0391427241948519,0.345585692469776,
-5.15678737160167));
#29526=CARTESIAN_POINT('Ctrl Pts',(-0.31165969221056,0.15436923251875,-5.14090178617716));
#29527=CARTESIAN_POINT('Ctrl Pts',(-0.298623247450242,-0.178285669024407,
-5.12501620075266));
#29528=CARTESIAN_POINT('Ctrl Pts',(-0.0119778324735712,-0.347589060855552,
-5.10913061532816));
#29529=CARTESIAN_POINT('Ctrl Pts',(0.285642087791955,-0.198419306971529,
-5.09324502990364));
#29530=CARTESIAN_POINT('Ctrl Pts',(0.321546826274025,0.132549093585398,
-5.07735944447914));
#29531=CARTESIAN_POINT('Ctrl Pts',(0.0628392170425058,0.342071420172299,
-5.06147385905463));
#29532=CARTESIAN_POINT('Ctrl Pts',(-0.253443860981231,0.238176054690927,
-5.04558827363013));
#29533=CARTESIAN_POINT('Ctrl Pts',(-0.337512888682964,-0.0839444677753746,
-5.02970268820562));
#29534=CARTESIAN_POINT('Ctrl Pts',(-0.112340908875126,-0.329152159176147,
-5.01381710278111));
#29535=CARTESIAN_POINT('Ctrl Pts',(0.215761705613502,-0.272779233241759,
-4.99793151735661));
#29536=CARTESIAN_POINT('Ctrl Pts',(0.346175966669865,0.0335234812839203,
-4.9820459319321));
#29537=CARTESIAN_POINT('Ctrl Pts',(0.159411807884773,0.309110820263732,
-4.9661603465076));
#29538=CARTESIAN_POINT('Ctrl Pts',(-0.173410974828944,0.301480111294401,
-4.95027476108308));
#29539=CARTESIAN_POINT('Ctrl Pts',(-0.347348611619563,0.0176228744298602,
-4.93438917565858));
#29540=CARTESIAN_POINT('Ctrl Pts',(-0.203033410619501,-0.282381050832776,
-4.91850359023406));
#29541=CARTESIAN_POINT('Ctrl Pts',(0.127308038750163,-0.323657669408275,
-4.90261800480957));
#29542=CARTESIAN_POINT('Ctrl Pts',(0.341005450255696,-0.0683879126243729,
-4.88673241938505));
#29543=CARTESIAN_POINT('Ctrl Pts',(0.24226184827928,0.249541220173173,-4.87084683396055));
#29544=CARTESIAN_POINT('Ctrl Pts',(-0.0784504563898112,0.3388320374307,
-4.85496124853604));
#29545=CARTESIAN_POINT('Ctrl Pts',(-0.327283733658682,0.117673197371545,
-4.83907566311153));
#29546=CARTESIAN_POINT('Ctrl Pts',(-0.276248309815004,-0.211301904917024,
-4.82319007768704));
#29547=CARTESIAN_POINT('Ctrl Pts',(0.0278953908217769,-0.346674877757401,
-4.80730449226252));
#29548=CARTESIAN_POINT('Ctrl Pts',(0.306480367475419,-0.164412311124628,
-4.79141890683802));
#29549=CARTESIAN_POINT('Ctrl Pts',(0.304257408201531,0.168490513832963,
-4.77553332141351));
#29550=CARTESIAN_POINT('Ctrl Pts',(0.0232632653392378,0.347016489785378,
-4.759647735989));
#29551=CARTESIAN_POINT('Ctrl Pts',(-0.279045487579995,0.207593929483624,
-4.7437621505645));
#29552=CARTESIAN_POINT('Ctrl Pts',(-0.325683092481844,-0.122033384648102,
-4.72787656513998));
#29553=CARTESIAN_POINT('Ctrl Pts',(-0.0739185591989158,-0.339849481834481,
-4.71199097971549));
#29554=CARTESIAN_POINT('Ctrl Pts',(0.24557272019296,-0.246283703874696,
-4.69610539429097));
#29555=CARTESIAN_POINT('Ctrl Pts',(0.340061761283145,0.072935740280159,
-4.68021980886648));
#29556=CARTESIAN_POINT('Ctrl Pts',(0.122974429438251,0.325328931085979,
-4.66433422344196));
#29557=CARTESIAN_POINT('Ctrl Pts',(-0.206786337207292,0.279644478653881,
-4.64844863801746));
#29558=CARTESIAN_POINT('Ctrl Pts',(-0.347082294059265,-0.0222599381797678,
-4.63256305259294));
#29559=CARTESIAN_POINT('Ctrl Pts',(-0.169369422500422,-0.303769028077391,
-4.61667746716844));
#29560=CARTESIAN_POINT('Ctrl Pts',(0.163525584649523,-0.306954405184615,
-4.60079188174393));
#29561=CARTESIAN_POINT('Ctrl Pts',(0.346592783006926,-0.0288975165840105,
-4.58490629631943));
#29562=CARTESIAN_POINT('Ctrl Pts',(0.212099659947135,0.275636278358852,
-4.56902071089492));
#29563=CARTESIAN_POINT('Ctrl Pts',(-0.116726523371279,0.32762256094302,
-4.55313512547042));
#29564=CARTESIAN_POINT('Ctrl Pts',(-0.338603819993014,0.0794296971122733,
-4.5372495400459));
#29565=CARTESIAN_POINT('Ctrl Pts',(-0.250240560024966,-0.241539408411135,
-4.5213639546214));
#29566=CARTESIAN_POINT('Ctrl Pts',(0.0674017748958896,-0.341201735690329,
-4.50547836919689));
#29567=CARTESIAN_POINT('Ctrl Pts',(0.323288267371518,-0.128243205968701,
-4.48959278377238));
#29568=CARTESIAN_POINT('Ctrl Pts',(0.282966843438066,0.20221619423752,-4.47370719834787));
#29569=CARTESIAN_POINT('Ctrl Pts',(-0.0166186106722786,0.34739810804973,
-4.45782161292338));
#29570=CARTESIAN_POINT('Ctrl Pts',(-0.300977517649094,0.174281833726291,
-4.44193602749886));
#29571=CARTESIAN_POINT('Ctrl Pts',(-0.30957039044947,-0.158517497627776,
-4.42605044207436));
#29572=CARTESIAN_POINT('Ctrl Pts',(-0.0345241411668705,-0.34607760310933,
-4.41016485664984));
#29573=CARTESIAN_POINT('Ctrl Pts',(0.272154322931305,-0.216549412853076,
-4.39427927122535));
#29574=CARTESIAN_POINT('Ctrl Pts',(0.329475562925319,0.111388855511911,
-4.37839368580083));
#29575=CARTESIAN_POINT('Ctrl Pts',(0.0849198718593337,0.337268793487633,
-4.36250810037633));
#29576=CARTESIAN_POINT('Ctrl Pts',(-0.237442349303437,0.254131372432594,
-4.34662251495183));
#29577=CARTESIAN_POINT('Ctrl Pts',(-0.34225165978905,-0.0618500207667643,
-4.33073692952732));
#29578=CARTESIAN_POINT('Ctrl Pts',(-0.133478136422044,-0.321162281089338,
-4.31485134410281));
#29579=CARTESIAN_POINT('Ctrl Pts',(0.19759268216448,-0.286214527325668,
-4.2989657586783));
#29580=CARTESIAN_POINT('Ctrl Pts',(0.347622236378851,0.0109728971641897,
-4.28308017325379));
#29581=CARTESIAN_POINT('Ctrl Pts',(0.179148248313675,0.298106572928794,
-4.26719458782929));
#29582=CARTESIAN_POINT('Ctrl Pts',(-0.15346757450713,0.312104673582609,
-4.25130900240478));
#29583=CARTESIAN_POINT('Ctrl Pts',(-0.345471086059395,0.0401416541033478,
-4.23542341698027));
#29584=CARTESIAN_POINT('Ctrl Pts',(-0.220942013818134,-0.268600540258568,
-4.21953783155577));
#29585=CARTESIAN_POINT('Ctrl Pts',(0.106021789792706,-0.331241609382573,
-4.20365224613125));
#29586=CARTESIAN_POINT('Ctrl Pts',(0.335844754659909,-0.0903876344676083,
-4.18776666070676));
#29587=CARTESIAN_POINT('Ctrl Pts',(0.257955114230381,0.233282624169873,
-4.17188107528224));
#29588=CARTESIAN_POINT('Ctrl Pts',(-0.0562819431172887,0.34321125648226,
-4.15599548985774));
#29589=CARTESIAN_POINT('Ctrl Pts',(-0.318951533332058,0.138677839190145,
-4.14010990443324));
#29590=CARTESIAN_POINT('Ctrl Pts',(-0.289386673184354,-0.192917021230238,
-4.12422431900872));
#29591=CARTESIAN_POINT('Ctrl Pts',(0.00532428767735682,-0.347754619894331,
-4.10833873358422));
#29592=CARTESIAN_POINT('Ctrl Pts',(0.295156951620275,-0.183967381913722,
-4.09245314815971));
#29593=CARTESIAN_POINT('Ctrl Pts',(0.314556585731257,0.14837714806886,-4.07656756273521));
#29594=CARTESIAN_POINT('Ctrl Pts',(0.0457485728179687,0.344773391928874,
-4.0606819773107));
#29595=CARTESIAN_POINT('Ctrl Pts',(-0.264975868266788,0.225276303544235,
-4.04479639188619));
#29596=CARTESIAN_POINT('Ctrl Pts',(-0.33292023420213,-0.10062674269826,
-4.02891080646169));
#29597=CARTESIAN_POINT('Ctrl Pts',(-0.0958315419103227,-0.334332079337508,
-4.01302522103718));
#29598=CARTESIAN_POINT('Ctrl Pts',(0.229061330908633,-0.261710776264314,
-3.99713963561267));
#29599=CARTESIAN_POINT('Ctrl Pts',(0.344080272397588,0.0506990115029886,
-3.98125405018816));
#29600=CARTESIAN_POINT('Ctrl Pts',(0.143840942183751,0.316656607518357,
-3.96536846476366));
#29601=CARTESIAN_POINT('Ctrl Pts',(-0.188190445868226,0.292482443903425,
-3.94948287933915));
#29602=CARTESIAN_POINT('Ctrl Pts',(-0.347795222829602,0.000325726836706584,
-3.93359729391464));
#29603=CARTESIAN_POINT('Ctrl Pts',(-0.188737964255785,-0.292129431872098,
-3.91771170849014));
#29604=CARTESIAN_POINT('Ctrl Pts',(0.143247564876018,-0.316925480399863,
-3.90182612306563));
#29605=CARTESIAN_POINT('Ctrl Pts',(0.343984698876466,-0.0513434163372087,
-3.88594053764113));
#29606=CARTESIAN_POINT('Ctrl Pts',(0.229551149674784,0.261281261283245,
-3.87005495221662));
#29607=CARTESIAN_POINT('Ctrl Pts',(-0.0952051604262189,0.334510998804856,
-3.85416936679211));
#29608=CARTESIAN_POINT('Ctrl Pts',(-0.332731123583902,0.101250148833917,
-3.83828378136761));
#29609=CARTESIAN_POINT('Ctrl Pts',(-0.265397450764868,-0.224779567000631,
-3.8223981959431));
#29610=CARTESIAN_POINT('Ctrl Pts',(0.045102860632521,-0.344858510282622,
-3.80651261051859));
#29611=CARTESIAN_POINT('Ctrl Pts',(0.31427779764301,-0.14896602070837,-3.79062702509408));
#29612=CARTESIAN_POINT('Ctrl Pts',(0.295501624885664,0.18341408360049,-3.77474143966957));
#29613=CARTESIAN_POINT('Ctrl Pts',(0.00597449078588094,0.347744266258115,
-3.75885585424507));
#29614=CARTESIAN_POINT('Ctrl Pts',(-0.289022562023056,0.19345828826664,
-3.74297026882056));
#29615=CARTESIAN_POINT('Ctrl Pts',(-0.319215082650408,-0.138079312779645,
-3.72708468339606));
#29616=CARTESIAN_POINT('Ctrl Pts',(-0.0569162995882634,-0.343106888837962,
-3.71119909797154));
#29617=CARTESIAN_POINT('Ctrl Pts',(0.257501441669556,-0.233762188635379,
-3.69531351254704));
#29618=CARTESIAN_POINT('Ctrl Pts',(0.336044900769636,0.0897522187464598,
-3.67942792712253));
#29619=CARTESIAN_POINT('Ctrl Pts',(0.10658126864456,0.33105441587802,-3.66354234169803));
#29620=CARTESIAN_POINT('Ctrl Pts',(-0.220320727040801,0.268990613013312,
-3.64765675627352));
#29621=CARTESIAN_POINT('Ctrl Pts',(-0.345776258125757,-0.0394479644336986,
-3.63177117084901));
#29622=CARTESIAN_POINT('Ctrl Pts',(-0.153577823762402,-0.311920926252076,
-3.61588558542451));
#29623=CARTESIAN_POINT('Ctrl Pts',(0.0670764293281557,-0.302713317039253,
-3.6052951951415));
#29624=CARTESIAN_POINT('Ctrl Pts',(0.151068846355364,-0.252451665989471,
-3.6));
#29625=CARTESIAN_POINT('Ctrl Pts',(0.159774743137966,-0.224059110187412,
-5.98774893273369));
#29626=CARTESIAN_POINT('Ctrl Pts',(0.234320760284833,-0.170900947006113,
-5.98245373759219));
#29627=CARTESIAN_POINT('Ctrl Pts',(0.32488003225337,0.0147687036258942,
-5.97186334730919));
#29628=CARTESIAN_POINT('Ctrl Pts',(0.163354453713877,0.281580260548018,
-5.95597776188468));
#29629=CARTESIAN_POINT('Ctrl Pts',(-0.148004964470583,0.289610074258948,
-5.94009217646017));
#29630=CARTESIAN_POINT('Ctrl Pts',(-0.323671898168684,0.0326796130970632,
-5.92420659103566));
#29631=CARTESIAN_POINT('Ctrl Pts',(-0.20282360260777,-0.25439330273973,
-5.90832100561116));
#29632=CARTESIAN_POINT('Ctrl Pts',(0.103881577158279,-0.308278831742322,
-5.89243542018665));
#29633=CARTESIAN_POINT('Ctrl Pts',(0.315395022308329,-0.0797620994888713,
-5.87654983476214));
#29634=CARTESIAN_POINT('Ctrl Pts',(0.237938737837567,0.221863105115123,
-5.86066424933764));
#29635=CARTESIAN_POINT('Ctrl Pts',(-0.057528433066161,0.320195326115013,
-5.84477866391313));
#29636=CARTESIAN_POINT('Ctrl Pts',(-0.30028442083838,0.125160897558301,
-5.82889307848862));
#29637=CARTESIAN_POINT('Ctrl Pts',(-0.267910261568841,-0.184554115754993,
-5.81300749306412));
#29638=CARTESIAN_POINT('Ctrl Pts',(0.00993300430809844,-0.325172268588677,
-5.7971219076396));
#29639=CARTESIAN_POINT('Ctrl Pts',(0.27867508040525,-0.167857343527245,
-5.78123632221511));
#29640=CARTESIAN_POINT('Ctrl Pts',(0.292085505786177,0.143254828639967,
-5.76535073679059));
#29641=CARTESIAN_POINT('Ctrl Pts',(0.0378770057315835,0.323111686739128,
-5.74946515136609));
#29642=CARTESIAN_POINT('Ctrl Pts',(-0.251035688443259,0.206922559772916,
-5.73357956594158));
#29643=CARTESIAN_POINT('Ctrl Pts',(-0.309940799706874,-0.0988562623142354,
-5.71769398051708));
#29644=CARTESIAN_POINT('Ctrl Pts',(-0.0848673986747166,-0.314059512283639,
-5.70180839509257));
#29645=CARTESIAN_POINT('Ctrl Pts',(0.217964450351541,-0.241510570814654,
-5.68592280966806));
#29646=CARTESIAN_POINT('Ctrl Pts',(0.321089717116476,0.0523187370704123,
-5.67003722424356));
#29647=CARTESIAN_POINT('Ctrl Pts',(0.13002145425739,0.298211799309964,-5.65415163881905));
#29648=CARTESIAN_POINT('Ctrl Pts',(-0.180176971203471,0.270872877105102,
-5.63826605339454));
#29649=CARTESIAN_POINT('Ctrl Pts',(-0.325291010651212,-0.00464916552977893,
-5.62238046797003));
#29650=CARTESIAN_POINT('Ctrl Pts',(-0.172362150716446,-0.275911480827357,
-5.60649488254553));
#29651=CARTESIAN_POINT('Ctrl Pts',(0.138490886051659,-0.294374134102762,
-5.59060929712103));
#29652=CARTESIAN_POINT('Ctrl Pts',(0.322453772680454,-0.0431210018986964,
-5.5747237116965));
#29653=CARTESIAN_POINT('Ctrl Pts',(0.2109733358391,0.247641086807527,-5.55883812627201));
#29654=CARTESIAN_POINT('Ctrl Pts',(-0.0938081840608051,0.311505828078151,
-5.54295254084749));
#29655=CARTESIAN_POINT('Ctrl Pts',(-0.312639394143541,0.0899581321970818,
-5.527066955423));
#29656=CARTESIAN_POINT('Ctrl Pts',(-0.245019554577654,-0.214012322524808,
-5.51118136999848));
#29657=CARTESIAN_POINT('Ctrl Pts',(0.04709569377771,-0.321897269244784,
-5.49529578457399));
#29658=CARTESIAN_POINT('Ctrl Pts',(0.296060235060131,-0.134848780250535,
-5.47941019914947));
#29659=CARTESIAN_POINT('Ctrl Pts',(0.273764126916927,0.175752835346323,
-5.46352461372497));
#29660=CARTESIAN_POINT('Ctrl Pts',(0.000635836459002592,0.325323611241308,
-5.44763902830045));
#29661=CARTESIAN_POINT('Ctrl Pts',(-0.273075029402188,0.176821618123943,
-5.43175344287596));
#29662=CARTESIAN_POINT('Ctrl Pts',(-0.296585087976933,-0.133690470523117,
-5.41586785745144));
#29663=CARTESIAN_POINT('Ctrl Pts',(-0.0483536086916446,-0.321710716087453,
-5.39998227202694));
#29664=CARTESIAN_POINT('Ctrl Pts',(0.244181122913523,-0.214968452410302,
-5.38409668660243));
#29665=CARTESIAN_POINT('Ctrl Pts',(0.312988645880066,0.0887353586184989,
-5.36821110117792));
#29666=CARTESIAN_POINT('Ctrl Pts',(0.0950251226542888,0.311136758329086,
-5.35232551575342));
#29667=CARTESIAN_POINT('Ctrl Pts',(-0.210003711715611,0.248463875411818,
-5.33643993032891));
#29668=CARTESIAN_POINT('Ctrl Pts',(-0.322619866246528,-0.0418602224321043,
-5.3205543449044));
#29669=CARTESIAN_POINT('Ctrl Pts',(-0.139640516647252,-0.293830533521418,
-5.3046687594799));
#29670=CARTESIAN_POINT('Ctrl Pts',(0.171282314534783,-0.276583125021395,
-5.28878317405539));
#29671=CARTESIAN_POINT('Ctrl Pts',(0.325270352139021,-0.00592067043078219,
-5.27289758863089));
#29672=CARTESIAN_POINT('Ctrl Pts',(0.181234418567013,0.270166507631257,
-5.25701200320637));
#29673=CARTESIAN_POINT('Ctrl Pts',(-0.128854771257734,0.298717766868846,
-5.24112641778187));
#29674=CARTESIAN_POINT('Ctrl Pts',(-0.32088275328195,0.0535734539225178,
-5.22524083235736));
#29675=CARTESIAN_POINT('Ctrl Pts',(-0.218906834286065,-0.240656714474884,
-5.20935524693286));
#29676=CARTESIAN_POINT('Ctrl Pts',(0.0836391140485833,-0.314388859408473,
-5.19346966150835));
#29677=CARTESIAN_POINT('Ctrl Pts',(0.309552006986385,-0.100067033980699,
-5.17758407608384));
#29678=CARTESIAN_POINT('Ctrl Pts',(0.251842621407298,0.205939676511578,
-5.16169849065934));
#29679=CARTESIAN_POINT('Ctrl Pts',(-0.0366137032938643,0.323257317086716,
-5.14581290523483));
#29680=CARTESIAN_POINT('Ctrl Pts',(-0.29152328393013,0.14439539897651,-5.12992731981032));
#29681=CARTESIAN_POINT('Ctrl Pts',(-0.279329127026664,-0.166766588720627,
-5.11404173438582));
#29682=CARTESIAN_POINT('Ctrl Pts',(-0.0112039418132435,-0.325131247355339,
-5.09815614896131));
#29683=CARTESIAN_POINT('Ctrl Pts',(0.267186683241381,-0.185599387438274,
-5.0822705635368));
#29684=CARTESIAN_POINT('Ctrl Pts',(0.300771607864467,0.123985064510271,
-5.0663849781123));
#29685=CARTESIAN_POINT('Ctrl Pts',(0.0587791599930511,0.319970102774469,
-5.05049939268778));
#29686=CARTESIAN_POINT('Ctrl Pts',(-0.237068791671855,0.222787442047884,
-5.03461380726328));
#29687=CARTESIAN_POINT('Ctrl Pts',(-0.315706099109945,-0.0785207953587747,
-5.01872822183877));
#29688=CARTESIAN_POINT('Ctrl Pts',(-0.105082535513916,-0.307885558363752,
-5.00284263641427));
#29689=CARTESIAN_POINT('Ctrl Pts',(0.201821289499056,-0.255154900842471,
-4.98695705098976));
#29690=CARTESIAN_POINT('Ctrl Pts',(0.323809453527616,0.0313575210298802,
-4.97107146556525));
#29691=CARTESIAN_POINT('Ctrl Pts',(0.149112172325483,0.2891390952178,-4.95518588014075));
#29692=CARTESIAN_POINT('Ctrl Pts',(-0.162206849699077,0.282001408205161,
-4.93930029471624));
#29693=CARTESIAN_POINT('Ctrl Pts',(-0.324906333602788,0.016484256240009,
-4.92341470929174));
#29694=CARTESIAN_POINT('Ctrl Pts',(-0.189915372730789,-0.264136342670823,
-4.90752912386722));
#29695=CARTESIAN_POINT('Ctrl Pts',(0.119082635498715,-0.302746068912006,
-4.89164353844272));
#29696=CARTESIAN_POINT('Ctrl Pts',(0.318973005432638,-0.0639693530080066,
-4.87575795301821));
#29697=CARTESIAN_POINT('Ctrl Pts',(0.22660925152183,0.233418301432662,-4.8598723675937));
#29698=CARTESIAN_POINT('Ctrl Pts',(-0.0733817533809408,0.316940017337243,
-4.8439867821692));
#29699=CARTESIAN_POINT('Ctrl Pts',(-0.306137852271999,0.110070303557685,
-4.82810119674469));
#29700=CARTESIAN_POINT('Ctrl Pts',(-0.258399839537187,-0.197649637606924,
-4.81221561132018));
#29701=CARTESIAN_POINT('Ctrl Pts',(0.0260930628571135,-0.324276129848818,
-4.79633002589568));
#29702=CARTESIAN_POINT('Ctrl Pts',(0.286678596621933,-0.153789591838562,
-4.78044444047117));
#29703=CARTESIAN_POINT('Ctrl Pts',(0.284599263285723,0.157604300881088,
-4.76455885504666));
#29704=CARTESIAN_POINT('Ctrl Pts',(0.0217602201251315,0.324595670240839,
-4.74867326962215));
#29705=CARTESIAN_POINT('Ctrl Pts',(-0.261016290968563,0.194181235365333,
-4.73278768419765));
#29706=CARTESIAN_POINT('Ctrl Pts',(-0.304640628909697,-0.11414877807711,
-4.71690209877314));
#29707=CARTESIAN_POINT('Ctrl Pts',(-0.0691426631663777,-0.3178917244114,
-4.70101651334863));
#29708=CARTESIAN_POINT('Ctrl Pts',(0.229706207198394,-0.230371254052065,
-4.68513092792413));
#29709=CARTESIAN_POINT('Ctrl Pts',(0.318090288433415,0.0682233444162613,
-4.66924534249962));
#29710=CARTESIAN_POINT('Ctrl Pts',(0.115029021735197,0.30430934996749,-4.65335975707511));
#29711=CARTESIAN_POINT('Ctrl Pts',(-0.193425821821788,0.261576581083932,
-4.63747417165061));
#29712=CARTESIAN_POINT('Ctrl Pts',(-0.324657222884633,-0.0208217181767073,
-4.6215885862261));
#29713=CARTESIAN_POINT('Ctrl Pts',(-0.158426423046438,-0.284142437519818,
-4.6057030008016));
#29714=CARTESIAN_POINT('Ctrl Pts',(0.152960156976014,-0.287122006639801,
-4.58981741537708));
#29715=CARTESIAN_POINT('Ctrl Pts',(0.324199339260075,-0.0270304410308685,
-4.57393182995258));
#29716=CARTESIAN_POINT('Ctrl Pts',(0.198395849491113,0.257827351581814,
-4.55804624452807));
#29717=CARTESIAN_POINT('Ctrl Pts',(-0.109184794394113,0.306454787843342,
-4.54216065910356));
#29718=CARTESIAN_POINT('Ctrl Pts',(-0.31672654508354,0.0742977251228926,
-4.52627507367906));
#29719=CARTESIAN_POINT('Ctrl Pts',(-0.234072456767065,-0.225933488668732,
-4.51038948825454));
#29720=CARTESIAN_POINT('Ctrl Pts',(0.0630469298772648,-0.319156608817747,
-4.49450390283005));
#29721=CARTESIAN_POINT('Ctrl Pts',(0.302400534030411,-0.119957381336518,
-4.47861831740553));
#29722=CARTESIAN_POINT('Ctrl Pts',(0.264684287073851,0.189150956897394,
-4.46273273198104));
#29723=CARTESIAN_POINT('Ctrl Pts',(-0.0155448782073034,0.324952632056601,
-4.44684714655652));
#29724=CARTESIAN_POINT('Ctrl Pts',(-0.281531287257139,0.163021442191914,
-4.43096156113202));
#29725=CARTESIAN_POINT('Ctrl Pts',(-0.289568972462407,-0.14827564367103,
-4.41507597570751));
#29726=CARTESIAN_POINT('Ctrl Pts',(-0.0322935280351681,-0.323717445260577,
-4.399190390283));
#29727=CARTESIAN_POINT('Ctrl Pts',(0.254570366138695,-0.202558102782889,
-4.3833048048585));
#29728=CARTESIAN_POINT('Ctrl Pts',(0.308188066918276,0.104191994549338,
-4.36741921943399));
#29729=CARTESIAN_POINT('Ctrl Pts',(0.0794331783483678,0.31547777496437,
-4.35153363400948));
#29730=CARTESIAN_POINT('Ctrl Pts',(-0.222101141543377,0.237711882841648,
-4.33564804858498));
#29731=CARTESIAN_POINT('Ctrl Pts',(-0.320138697065879,-0.0578538759285308,
-4.31976246316047));
#29732=CARTESIAN_POINT('Ctrl Pts',(-0.12485408166398,-0.300411908237402,
-4.30387687773596));
#29733=CARTESIAN_POINT('Ctrl Pts',(0.184826171060436,-0.267722137318025,
-4.28799129231145));
#29734=CARTESIAN_POINT('Ctrl Pts',(0.325162279400034,0.0102639356178628,
-4.27210570688695));
#29735=CARTESIAN_POINT('Ctrl Pts',(0.167573436552869,0.278845834971323,
-4.25622012146245));
#29736=CARTESIAN_POINT('Ctrl Pts',(-0.143551997307641,0.291939514947838,
-4.24033453603793));
#29737=CARTESIAN_POINT('Ctrl Pts',(-0.323150115424298,0.0375480920987667,
-4.22444895061343));
#29738=CARTESIAN_POINT('Ctrl Pts',(-0.206666896734541,-0.251246194226113,
-4.20856336518893));
#29739=CARTESIAN_POINT('Ctrl Pts',(0.0991716962475789,-0.309840008685721,
-4.19267777976441));
#29740=CARTESIAN_POINT('Ctrl Pts',(0.314145743630585,-0.0845476674887783,
-4.17679219433991));
#29741=CARTESIAN_POINT('Ctrl Pts',(0.241288571754755,0.218210177259282,
-4.16090660891539));
#29742=CARTESIAN_POINT('Ctrl Pts',(-0.0526455531260544,0.321036293984072,
-4.1450210234909));
#29743=CARTESIAN_POINT('Ctrl Pts',(-0.298343997428749,0.129717830375486,
-4.12913543806638));
#29744=CARTESIAN_POINT('Ctrl Pts',(-0.270689330063645,-0.180452605712841,
-4.11324985264189));
#29745=CARTESIAN_POINT('Ctrl Pts',(0.00498028415956703,-0.32528610958448,
-4.09736426721737));
#29746=CARTESIAN_POINT('Ctrl Pts',(0.276086789410728,-0.172081204762544,
-4.08147868179287));
#29747=CARTESIAN_POINT('Ctrl Pts',(0.294233008458059,0.138790464555801,
-4.06559309636836));
#29748=CARTESIAN_POINT('Ctrl Pts',(0.0427927464357516,0.322497499480716,
-4.04970751094385));
#29749=CARTESIAN_POINT('Ctrl Pts',(-0.247855713170579,0.210721146950524,
-4.03382192551934));
#29750=CARTESIAN_POINT('Ctrl Pts',(-0.311410177148678,-0.0941252244540177,
-4.01793634009484));
#29751=CARTESIAN_POINT('Ctrl Pts',(-0.0896398427516596,-0.312730802627535,
-4.00205075467033));
#29752=CARTESIAN_POINT('Ctrl Pts',(0.214261622779169,-0.244801579554058,
-3.98616516924583));
#29753=CARTESIAN_POINT('Ctrl Pts',(0.321849162570404,0.0474233360770221,
-3.97027958382132));
#29754=CARTESIAN_POINT('Ctrl Pts',(0.134547344032802,0.296197347328312,
-3.95439399839681));
#29755=CARTESIAN_POINT('Ctrl Pts',(-0.176031415531,0.273585082285939,-3.93850841297231));
#29756=CARTESIAN_POINT('Ctrl Pts',(-0.325324089154259,0.000304681546809577,
-3.9226228275478));
#29757=CARTESIAN_POINT('Ctrl Pts',(-0.176543558622785,-0.273254878447549,
-3.90673724212329));
#29758=CARTESIAN_POINT('Ctrl Pts',(0.133992304976795,-0.29644884826775,
-3.89085165669878));
#29759=CARTESIAN_POINT('Ctrl Pts',(0.321759764077655,-0.048026105758658,
-3.87496607127428));
#29760=CARTESIAN_POINT('Ctrl Pts',(0.214719794236075,0.244399815640059,
-3.85908048584977));
#29761=CARTESIAN_POINT('Ctrl Pts',(-0.0890539319271196,0.312898162064716,
-3.84319490042526));
#29762=CARTESIAN_POINT('Ctrl Pts',(-0.311233285013347,0.0947083521680955,
-3.82730931500076));
#29763=CARTESIAN_POINT('Ctrl Pts',(-0.248250057121239,-0.210256504675443,
-3.81142372957625));
#29764=CARTESIAN_POINT('Ctrl Pts',(0.0421887538711686,-0.32257711831699,
-3.79553814415174));
#29765=CARTESIAN_POINT('Ctrl Pts',(0.29397223293579,-0.13934128999129,-3.77965255872724));
#29766=CARTESIAN_POINT('Ctrl Pts',(0.276409193252869,0.171563655187485,
-3.76376697330273));
#29767=CARTESIAN_POINT('Ctrl Pts',(0.00558847748759769,0.325276424899211,
-3.74788138787822));
#29768=CARTESIAN_POINT('Ctrl Pts',(-0.270348744212762,0.180958901354783,
-3.73199580245371));
#29769=CARTESIAN_POINT('Ctrl Pts',(-0.298590518761739,-0.12915797490149,
-3.71611021702921));
#29770=CARTESIAN_POINT('Ctrl Pts',(-0.0532389236716297,-0.320938669558577,
-3.7002246316047));
#29771=CARTESIAN_POINT('Ctrl Pts',(0.240864211088085,-0.218658756948394,
-3.68433904618019));
#29772=CARTESIAN_POINT('Ctrl Pts',(0.314332958251634,0.0839533061314393,
-3.66845346075569));
#29773=CARTESIAN_POINT('Ctrl Pts',(0.0996950270351602,0.309664909798885,
-3.65256787533118));
#29774=CARTESIAN_POINT('Ctrl Pts',(-0.206085751446533,0.251611064285594,
-3.63668228990667));
#29775=CARTESIAN_POINT('Ctrl Pts',(-0.323435570249458,-0.0368992218868692,
-3.62079670448217));
#29776=CARTESIAN_POINT('Ctrl Pts',(-0.143655123331798,-0.291767639576884,
-3.60491111905766));
#29777=CARTESIAN_POINT('Ctrl Pts',(0.0627426049655472,-0.283154936227829,
-3.59432072877466));
#29778=CARTESIAN_POINT('Ctrl Pts',(0.141308251563369,-0.236140702639086,
-3.58902553363315));
#29779=CARTESIAN_POINT('Ctrl Pts',(0.148738611075533,-0.208582659521589,
-5.97677446636685));
#29780=CARTESIAN_POINT('Ctrl Pts',(0.218135505940597,-0.159096293881898,
-5.97147927122534));
#29781=CARTESIAN_POINT('Ctrl Pts',(0.302439570951552,0.0137485839223339,
-5.96088888094234));
#29782=CARTESIAN_POINT('Ctrl Pts',(0.152071060051237,0.2621306474205,-5.94500329551783));
#29783=CARTESIAN_POINT('Ctrl Pts',(-0.137781807157274,0.269605817244605,
-5.92911771009332));
#29784=CARTESIAN_POINT('Ctrl Pts',(-0.30131488639741,0.0304223318847445,
-5.91323212466882));
#29785=CARTESIAN_POINT('Ctrl Pts',(-0.188813953649519,-0.236821576259721,
-5.89734653924431));
#29786=CARTESIAN_POINT('Ctrl Pts',(0.0967061576779765,-0.286985066330208,
-5.88146095381981));
#29787=CARTESIAN_POINT('Ctrl Pts',(0.293609719765092,-0.0742526863848491,
-5.8655753683953));
#29788=CARTESIAN_POINT('Ctrl Pts',(0.221503578675544,0.206538339262002,
-5.84968978297079));
#29789=CARTESIAN_POINT('Ctrl Pts',(-0.0535547675656337,0.298078451849551,
-5.83380419754629));
#29790=CARTESIAN_POINT('Ctrl Pts',(-0.279542853932516,0.116515650084404,
-5.81791861212177));
#29791=CARTESIAN_POINT('Ctrl Pts',(-0.249404877241599,-0.171806396346182,
-5.80203302669728));
#29792=CARTESIAN_POINT('Ctrl Pts',(0.00924690120339052,-0.302711621625931,
-5.78614744127276));
#29793=CARTESIAN_POINT('Ctrl Pts',(0.259426136989922,-0.156262921440043,
-5.77026185584826));
#29794=CARTESIAN_POINT('Ctrl Pts',(0.271910263115969,0.133359777792746,
-5.75437627042375));
#29795=CARTESIAN_POINT('Ctrl Pts',(0.0352607246525252,0.300793370491302,
-5.73849068499924));
#29796=CARTESIAN_POINT('Ctrl Pts',(-0.233695882691538,0.192629783258305,
-5.72260509957474));
#29797=CARTESIAN_POINT('Ctrl Pts',(-0.288532237064735,-0.0920279567593562,
-5.70671951415023));
#29798=CARTESIAN_POINT('Ctrl Pts',(-0.0790053468812083,-0.292366457518203,
-5.69083392872573));
#29799=CARTESIAN_POINT('Ctrl Pts',(0.20290897655292,-0.224828694182361,
-5.67494834330121));
#29800=CARTESIAN_POINT('Ctrl Pts',(0.298911064518509,0.0487049212675593,
-5.65906275787671));
#29801=CARTESIAN_POINT('Ctrl Pts',(0.121040473208996,0.277613394736605,
-5.6431771724522));
#29802=CARTESIAN_POINT('Ctrl Pts',(-0.167731594607913,0.252162855826698,
-5.6272915870277));
#29803=CARTESIAN_POINT('Ctrl Pts',(-0.302822161809634,-0.00432803339237701,
-5.61140600160319));
#29804=CARTESIAN_POINT('Ctrl Pts',(-0.160456567765648,-0.256853427719911,
-5.59552041617868));
#29805=CARTESIAN_POINT('Ctrl Pts',(0.128924895345672,-0.274040808847988,
-5.57963483075418));
#29806=CARTESIAN_POINT('Ctrl Pts',(0.300180900576644,-0.0401425019038163,
-5.56374924532967));
#29807=CARTESIAN_POINT('Ctrl Pts',(0.196400759784563,0.230535756613179,
-5.54786365990516));
#29808=CARTESIAN_POINT('Ctrl Pts',(-0.087328564769926,0.289989164121325,
-5.53197807448066));
#29809=CARTESIAN_POINT('Ctrl Pts',(-0.291044431298209,0.0837444478091843,
-5.51609248905615));
#29810=CARTESIAN_POINT('Ctrl Pts',(-0.228095301663273,-0.199229834329336,
-5.50020690363164));
#29811=CARTESIAN_POINT('Ctrl Pts',(0.043842649611312,-0.2996628365419,-5.48432131820714));
#29812=CARTESIAN_POINT('Ctrl Pts',(0.275610445635422,-0.125534360974531,
-5.46843573278262));
#29813=CARTESIAN_POINT('Ctrl Pts',(0.254854398137061,0.163613047397773,
-5.45255014735812));
#29814=CARTESIAN_POINT('Ctrl Pts',(0.000591917282580738,0.302852510576879,
-5.43666456193361));
#29815=CARTESIAN_POINT('Ctrl Pts',(-0.25421289870339,0.164608006067476,
-5.4207789765091));
#29816=CARTESIAN_POINT('Ctrl Pts',(-0.276099045349813,-0.124456059256326,
-5.4048933910846));
#29817=CARTESIAN_POINT('Ctrl Pts',(-0.0450136764799851,-0.299489169183916,
-5.38900780566009));
#29818=CARTESIAN_POINT('Ctrl Pts',(0.227314783048407,-0.200119921388048,
-5.37312222023559));
#29819=CARTESIAN_POINT('Ctrl Pts',(0.29136955914499,0.0826061349559363,
-5.35723663481108));
#29820=CARTESIAN_POINT('Ctrl Pts',(0.0884614456784106,0.289645587152977,
-5.34135104938657));
#29821=CARTESIAN_POINT('Ctrl Pts',(-0.195498110576304,0.231301712682376,
-5.32546546396206));
#29822=CARTESIAN_POINT('Ctrl Pts',(-0.300335521550154,-0.0389688083459327,
-5.30957987853756));
#29823=CARTESIAN_POINT('Ctrl Pts',(-0.129995117426334,-0.273534756427806,
-5.29369429311305));
#29824=CARTESIAN_POINT('Ctrl Pts',(0.159451319184456,-0.257478679387327,
-5.27780870768854));
#29825=CARTESIAN_POINT('Ctrl Pts',(0.302802930244308,-0.00551171154598658,
-5.26192312226404));
#29826=CARTESIAN_POINT('Ctrl Pts',(0.168716000835391,0.251505277461166,
-5.24603753683952));
#29827=CARTESIAN_POINT('Ctrl Pts',(-0.119954376586175,0.278084413562731,
-5.23015195141503));
#29828=CARTESIAN_POINT('Ctrl Pts',(-0.298718396311471,0.0498729709743527,
-5.21426636599051));
#29829=CARTESIAN_POINT('Ctrl Pts',(-0.2037862671357,-0.22403381632156,-5.19838078056602));
#29830=CARTESIAN_POINT('Ctrl Pts',(0.0778619036453848,-0.292673055625936,
-5.1824951951415));
#29831=CARTESIAN_POINT('Ctrl Pts',(0.288170299451153,-0.0931550967094044,
-5.166609609717));
#29832=CARTESIAN_POINT('Ctrl Pts',(0.234447078318237,0.191714790761558,
-5.15072402429248));
#29833=CARTESIAN_POINT('Ctrl Pts',(-0.0340846823928767,0.300928941703655,
-5.13483843886799));
#29834=CARTESIAN_POINT('Ctrl Pts',(-0.2713868756497,0.134421565434269,-5.11895285344347));
#29835=CARTESIAN_POINT('Ctrl Pts',(-0.260035006603086,-0.155247508416846,
-5.10306726801897));
#29836=CARTESIAN_POINT('Ctrl Pts',(-0.0104300511529157,-0.302673433855126,
-5.08718168259447));
#29837=CARTESIAN_POINT('Ctrl Pts',(0.248731278690807,-0.172779467905019,
-5.07129609716995));
#29838=CARTESIAN_POINT('Ctrl Pts',(0.279996389454909,0.115421035435144,
-5.05541051174546));
#29839=CARTESIAN_POINT('Ctrl Pts',(0.0547191029435964,0.297868785376638,
-5.03952492632093));
#29840=CARTESIAN_POINT('Ctrl Pts',(-0.22069372236248,0.207398829404841,
-5.02363934089644));
#29841=CARTESIAN_POINT('Ctrl Pts',(-0.293899309536927,-0.0730971229421753,
-5.00775375547193));
#29842=CARTESIAN_POINT('Ctrl Pts',(-0.0978241621527061,-0.286618957551357,
-4.99186817004742));
#29843=CARTESIAN_POINT('Ctrl Pts',(0.18788087338461,-0.237530568443184,
-4.97598258462292));
#29844=CARTESIAN_POINT('Ctrl Pts',(0.301442940385367,0.0291915607758403,
-4.9600969991984));
#29845=CARTESIAN_POINT('Ctrl Pts',(0.138812536766193,0.269167370171868,
-4.9442114137739));
#29846=CARTESIAN_POINT('Ctrl Pts',(-0.15100272456921,0.262522705115921,
-4.92832582834939));
#29847=CARTESIAN_POINT('Ctrl Pts',(-0.302464055586014,0.0153456380501578,
-4.91244024292488));
#29848=CARTESIAN_POINT('Ctrl Pts',(-0.176797334842078,-0.245891634508871,
-4.89655465750038));
#29849=CARTESIAN_POINT('Ctrl Pts',(0.110857232247267,-0.281834468415737,
-4.88066907207587));
#29850=CARTESIAN_POINT('Ctrl Pts',(0.29694056060958,-0.0595507933916408,
-4.86478348665137));
#29851=CARTESIAN_POINT('Ctrl Pts',(0.210956654764379,0.21729538269215,-4.84889790122686));
#29852=CARTESIAN_POINT('Ctrl Pts',(-0.0683130503720702,0.295047997243785,
-4.83301231580235));
#29853=CARTESIAN_POINT('Ctrl Pts',(-0.284991970885316,0.102467409743826,
-4.81712673037784));
#29854=CARTESIAN_POINT('Ctrl Pts',(-0.240551369259371,-0.183997370296825,
-4.80124114495333));
#29855=CARTESIAN_POINT('Ctrl Pts',(0.0242907348924498,-0.301877381940235,
-4.78535555952883));
#29856=CARTESIAN_POINT('Ctrl Pts',(0.266876825768449,-0.143166872552496,
-4.76946997410432));
#29857=CARTESIAN_POINT('Ctrl Pts',(0.264941118369915,0.146718087929213,
-4.75358438867982));
#29858=CARTESIAN_POINT('Ctrl Pts',(0.0202571749110258,0.302174850696298,
-4.73769880325531));
#29859=CARTESIAN_POINT('Ctrl Pts',(-0.242987094357132,0.180768541247043,
-4.72181321783081));
#29860=CARTESIAN_POINT('Ctrl Pts',(-0.283598165337549,-0.106264171506117,
-4.70592763240629));
#29861=CARTESIAN_POINT('Ctrl Pts',(-0.0643667671338396,-0.295933966988319,
-4.69004204698179));
#29862=CARTESIAN_POINT('Ctrl Pts',(0.213839694203828,-0.214458804229434,
-4.67415646155728));
#29863=CARTESIAN_POINT('Ctrl Pts',(0.296118815583686,0.0635109485523635,
-4.65827087613277));
#29864=CARTESIAN_POINT('Ctrl Pts',(0.107083614032142,0.283289768849002,
-4.64238529070827));
#29865=CARTESIAN_POINT('Ctrl Pts',(-0.180065306436283,0.243508683513982,
-4.62649970528376));
#29866=CARTESIAN_POINT('Ctrl Pts',(-0.302232151710002,-0.0193834981736465,
-4.61061411985926));
#29867=CARTESIAN_POINT('Ctrl Pts',(-0.147483423592454,-0.264515846962246,
-4.59472853443474));
#29868=CARTESIAN_POINT('Ctrl Pts',(0.142394729302505,-0.267289608094988,
-4.57884294901024));
#29869=CARTESIAN_POINT('Ctrl Pts',(0.301805895513226,-0.0251633654777264,
-4.56295736358573));
#29870=CARTESIAN_POINT('Ctrl Pts',(0.184692039035091,0.240018424804776,
-4.54707177816123));
#29871=CARTESIAN_POINT('Ctrl Pts',(-0.101643065416946,0.285287014743665,
-4.53118619273672));
#29872=CARTESIAN_POINT('Ctrl Pts',(-0.294849270174067,0.0691657531335122,
-4.51530060731221));
#29873=CARTESIAN_POINT('Ctrl Pts',(-0.217904353509163,-0.210327568926329,
-4.4994150218877));
#29874=CARTESIAN_POINT('Ctrl Pts',(0.0586920848586398,-0.297111481945164,
-4.4835294364632));
#29875=CARTESIAN_POINT('Ctrl Pts',(0.281512800689305,-0.111671556704335,
-4.46764385103869));
#29876=CARTESIAN_POINT('Ctrl Pts',(0.246401730709637,0.176085719557269,
-4.45175826561419));
#29877=CARTESIAN_POINT('Ctrl Pts',(-0.0144711457423287,0.302507156063472,
-4.43587268018968));
#29878=CARTESIAN_POINT('Ctrl Pts',(-0.262085056865184,0.151761050657536,
-4.41998709476516));
#29879=CARTESIAN_POINT('Ctrl Pts',(-0.269567554475346,-0.138033789714284,
-4.40410150934067));
#29880=CARTESIAN_POINT('Ctrl Pts',(-0.0300629149034655,-0.301357287411823,
-4.38821592391615));
#29881=CARTESIAN_POINT('Ctrl Pts',(0.236986409346085,-0.188566792712703,
-4.37233033849166));
#29882=CARTESIAN_POINT('Ctrl Pts',(0.286900570911232,0.0969951335867651,
-4.35644475306714));
#29883=CARTESIAN_POINT('Ctrl Pts',(0.0739464848374023,0.293686756441107,
-4.34055916764264));
#29884=CARTESIAN_POINT('Ctrl Pts',(-0.206759933783318,0.221292393250703,
-4.32467358221813));
#29885=CARTESIAN_POINT('Ctrl Pts',(-0.298025734342708,-0.0538577310902972,
-4.30878799679363));
#29886=CARTESIAN_POINT('Ctrl Pts',(-0.116230026905917,-0.279661535385465,
-4.29290241136911));
#29887=CARTESIAN_POINT('Ctrl Pts',(0.172059659956391,-0.249229747310381,
-4.27701682594461));
#29888=CARTESIAN_POINT('Ctrl Pts',(0.302702322421217,0.00955497407153588,
-4.2611312405201));
#29889=CARTESIAN_POINT('Ctrl Pts',(0.155998624792064,0.259585097013851,
-4.2452456550956));
#29890=CARTESIAN_POINT('Ctrl Pts',(-0.133636420108152,0.271774356313068,
-4.22936006967109));
#29891=CARTESIAN_POINT('Ctrl Pts',(-0.3008291447892,0.0349545300941856,
-4.21347448424658));
#29892=CARTESIAN_POINT('Ctrl Pts',(-0.192391779650948,-0.233891848193658,
-4.19758889882208));
#29893=CARTESIAN_POINT('Ctrl Pts',(0.0923216027024518,-0.288438407988869,
-4.18170331339757));
#29894=CARTESIAN_POINT('Ctrl Pts',(0.292446732601261,-0.0787077005099487,
-4.16581772797307));
#29895=CARTESIAN_POINT('Ctrl Pts',(0.224622029279129,0.203137730348692,
-4.14993214254855));
#29896=CARTESIAN_POINT('Ctrl Pts',(-0.0490091631348199,0.298861331485884,
-4.13404655712405));
#29897=CARTESIAN_POINT('Ctrl Pts',(-0.27773646152544,0.120757821560827,
-4.11816097169954));
#29898=CARTESIAN_POINT('Ctrl Pts',(-0.251991986942937,-0.167988190195444,
-4.10227538627504));
#29899=CARTESIAN_POINT('Ctrl Pts',(0.00463628064177704,-0.302817599274629,
-4.08638980085052));
#29900=CARTESIAN_POINT('Ctrl Pts',(0.257016627201181,-0.160195027611366,
-4.07050421542602));
#29901=CARTESIAN_POINT('Ctrl Pts',(0.273909431184861,0.12920378104274,-4.05461863000152));
#29902=CARTESIAN_POINT('Ctrl Pts',(0.0398369200535349,0.300221607032558,
-4.038733044577));
#29903=CARTESIAN_POINT('Ctrl Pts',(-0.230735558074371,0.196165990356812,
-4.0228474591525));
#29904=CARTESIAN_POINT('Ctrl Pts',(-0.289900120095227,-0.087623706209775,
-4.00696187372799));
#29905=CARTESIAN_POINT('Ctrl Pts',(-0.0834481435929966,-0.291129525917563,
-3.99107628830349));
#29906=CARTESIAN_POINT('Ctrl Pts',(0.199461914649706,-0.227892382843801,
-3.97519070287898));
#29907=CARTESIAN_POINT('Ctrl Pts',(0.29961805274322,0.0441476606510558,
-3.95930511745447));
#29908=CARTESIAN_POINT('Ctrl Pts',(0.125253745881852,0.275738087138265,
-3.94341953202996));
#29909=CARTESIAN_POINT('Ctrl Pts',(-0.163872385193774,0.254687720668454,
-3.92753394660546));
#29910=CARTESIAN_POINT('Ctrl Pts',(-0.302852955478915,0.000283636256912637,
-3.91164836118095));
#29911=CARTESIAN_POINT('Ctrl Pts',(-0.164349152989785,-0.254380325023001,
-3.89576277575645));
#29912=CARTESIAN_POINT('Ctrl Pts',(0.124737045077571,-0.275972216135638,
-3.87987719033194));
#29913=CARTESIAN_POINT('Ctrl Pts',(0.299534829278844,-0.0447087951801068,
-3.86399160490743));
#29914=CARTESIAN_POINT('Ctrl Pts',(0.199888438797366,0.227518369996871,
-3.84810601948293));
#29915=CARTESIAN_POINT('Ctrl Pts',(-0.0829027034280202,0.291285325324577,
-3.83222043405842));
#29916=CARTESIAN_POINT('Ctrl Pts',(-0.289735446442791,0.0881665555022742,
-3.81633484863391));
#29917=CARTESIAN_POINT('Ctrl Pts',(-0.231102663477611,-0.195733442350255,
-3.8004492632094));
#29918=CARTESIAN_POINT('Ctrl Pts',(0.0392746471098163,-0.300295726351358,
-3.78456367778489));
#29919=CARTESIAN_POINT('Ctrl Pts',(0.273666668228569,-0.12971655927421,
-3.76867809236039));
#29920=CARTESIAN_POINT('Ctrl Pts',(0.257316761620074,0.15971322677448,-3.75279250693588));
#29921=CARTESIAN_POINT('Ctrl Pts',(0.00520246418931447,0.302808583540306,
-3.73690692151138));
#29922=CARTESIAN_POINT('Ctrl Pts',(-0.251674926402469,0.168459514442926,
-3.72102133608687));
#29923=CARTESIAN_POINT('Ctrl Pts',(-0.27796595487307,-0.120236637023335,
-3.70513575066236));
#29924=CARTESIAN_POINT('Ctrl Pts',(-0.0495615477549964,-0.298770450279193,
-3.68925016523786));
#29925=CARTESIAN_POINT('Ctrl Pts',(0.224226980506614,-0.20355532526141,
-3.67336457981335));
#29926=CARTESIAN_POINT('Ctrl Pts',(0.292621015733633,0.0781543935164189,
-3.65747899438884));
#29927=CARTESIAN_POINT('Ctrl Pts',(0.0928087854257608,0.288275403719751,
-3.64159340896433));
#29928=CARTESIAN_POINT('Ctrl Pts',(-0.191850775852264,0.234231515557876,
-3.62570782353983));
#29929=CARTESIAN_POINT('Ctrl Pts',(-0.301094882373159,-0.0343504793400395,
-3.60982223811532));
#29930=CARTESIAN_POINT('Ctrl Pts',(-0.133732422901194,-0.271614352901692,
-3.59393665269081));
#29931=CARTESIAN_POINT('Ctrl Pts',(0.058408780602939,-0.263596555416404,
-3.58334626240781));
#29932=CARTESIAN_POINT('Ctrl Pts',(0.131547656771374,-0.219829739288701,
-3.57805106726631));
#29933=CARTESIAN_POINT('Ctrl Pts',(0.137702479013101,-0.193106208855765,
-5.9658));
#29934=CARTESIAN_POINT('Ctrl Pts',(0.201950251596361,-0.147291640757684,
-5.9605048048585));
#29935=CARTESIAN_POINT('Ctrl Pts',(0.279999109649734,0.0127284642187734,
-5.9499144145755));
#29936=CARTESIAN_POINT('Ctrl Pts',(0.140787666388597,0.242681034292982,
-5.93402882915098));
#29937=CARTESIAN_POINT('Ctrl Pts',(-0.127558649843965,0.249601560230261,
-5.91814324372648));
#29938=CARTESIAN_POINT('Ctrl Pts',(-0.278957874626137,0.0281650506724263,
-5.90225765830197));
#29939=CARTESIAN_POINT('Ctrl Pts',(-0.174804304691268,-0.219249849779713,
-5.88637207287746));
#29940=CARTESIAN_POINT('Ctrl Pts',(0.0895307381976737,-0.265691300918094,
-5.87048648745296));
#29941=CARTESIAN_POINT('Ctrl Pts',(0.271824417221856,-0.0687432732808278,
-5.85460090202845));
#29942=CARTESIAN_POINT('Ctrl Pts',(0.205068419513521,0.191213573408882,
-5.83871531660395));
#29943=CARTESIAN_POINT('Ctrl Pts',(-0.0495811020651061,0.275961577584089,
-5.82282973117944));
#29944=CARTESIAN_POINT('Ctrl Pts',(-0.258801287026652,0.107870402610509,
-5.80694414575493));
#29945=CARTESIAN_POINT('Ctrl Pts',(-0.230899492914356,-0.159058676937372,
-5.79105856033042));
#29946=CARTESIAN_POINT('Ctrl Pts',(0.00856079809868226,-0.280250974663184,
-5.77517297490592));
#29947=CARTESIAN_POINT('Ctrl Pts',(0.240177193574594,-0.144668499352843,
-5.75928738948141));
#29948=CARTESIAN_POINT('Ctrl Pts',(0.251735020445761,0.123464726945526,
-5.74340180405691));
#29949=CARTESIAN_POINT('Ctrl Pts',(0.0326444435734673,0.278475054243476,
-5.72751621863239));
#29950=CARTESIAN_POINT('Ctrl Pts',(-0.216356076939817,0.178337006743693,
-5.7116306332079));
#29951=CARTESIAN_POINT('Ctrl Pts',(-0.267123674422595,-0.0851996512044772,
-5.69574504778338));
#29952=CARTESIAN_POINT('Ctrl Pts',(-0.0731432950877003,-0.270673402752768,
-5.67985946235888));
#29953=CARTESIAN_POINT('Ctrl Pts',(0.187853502754299,-0.208146817550068,
-5.66397387693437));
#29954=CARTESIAN_POINT('Ctrl Pts',(0.276732411920541,0.0450911054647064,
-5.64808829150987));
#29955=CARTESIAN_POINT('Ctrl Pts',(0.112059492160603,0.257014990163246,
-5.63220270608536));
#29956=CARTESIAN_POINT('Ctrl Pts',(-0.155286218012354,0.233452834548294,
-5.61631712066085));
#29957=CARTESIAN_POINT('Ctrl Pts',(-0.280353312968057,-0.00400690125497473,
-5.60043153523634));
#29958=CARTESIAN_POINT('Ctrl Pts',(-0.14855098481485,-0.237795374612464,
-5.58454594981183));
#29959=CARTESIAN_POINT('Ctrl Pts',(0.119358904639683,-0.253707483593214,
-5.56866036438733));
#29960=CARTESIAN_POINT('Ctrl Pts',(0.277908028472834,-0.0371640019089366,
-5.55277477896282));
#29961=CARTESIAN_POINT('Ctrl Pts',(0.181828183730025,0.21343042641883,-5.53688919353832));
#29962=CARTESIAN_POINT('Ctrl Pts',(-0.0808489454790468,0.268472500164499,
-5.52100360811381));
#29963=CARTESIAN_POINT('Ctrl Pts',(-0.269449468452876,0.0775307634212869,
-5.5051180226893));
#29964=CARTESIAN_POINT('Ctrl Pts',(-0.211171048748891,-0.184447346133863,
-5.48923243726479));
#29965=CARTESIAN_POINT('Ctrl Pts',(0.040589605444914,-0.277428403839015,
-5.47334685184029));
#29966=CARTESIAN_POINT('Ctrl Pts',(0.255160656210713,-0.116219941698528,
-5.45746126641578));
#29967=CARTESIAN_POINT('Ctrl Pts',(0.235944669357195,0.151473259449223,
-5.44157568099128));
#29968=CARTESIAN_POINT('Ctrl Pts',(0.000547998106158669,0.280381409912451,
-5.42569009556676));
#29969=CARTESIAN_POINT('Ctrl Pts',(-0.235350768004592,0.152394394011009,
-5.40980451014226));
#29970=CARTESIAN_POINT('Ctrl Pts',(-0.255613002722693,-0.115221647989535,
-5.39391892471775));
#29971=CARTESIAN_POINT('Ctrl Pts',(-0.0416737442683253,-0.27726762228038,
-5.37803333929325));
#29972=CARTESIAN_POINT('Ctrl Pts',(0.21044844318329,-0.185271390365794,
-5.36214775386874));
#29973=CARTESIAN_POINT('Ctrl Pts',(0.269750472409913,0.0764769112933738,
-5.34626216844423));
#29974=CARTESIAN_POINT('Ctrl Pts',(0.0818977687025324,0.268154415976868,
-5.33037658301972));
#29975=CARTESIAN_POINT('Ctrl Pts',(-0.180992509436998,0.214139549952934,
-5.31449099759522));
#29976=CARTESIAN_POINT('Ctrl Pts',(-0.278051176853781,-0.0360773942597614,
-5.2986054121707));
#29977=CARTESIAN_POINT('Ctrl Pts',(-0.120349718205416,-0.253238979334194,
-5.28271982674621));
#29978=CARTESIAN_POINT('Ctrl Pts',(0.147620323834129,-0.23837423375326,
-5.2668342413217));
#29979=CARTESIAN_POINT('Ctrl Pts',(0.280335508349595,-0.00510275266119098,
-5.25094865589719));
#29980=CARTESIAN_POINT('Ctrl Pts',(0.156197583103769,0.232844047291076,
-5.23506307047268));
#29981=CARTESIAN_POINT('Ctrl Pts',(-0.111053981914616,0.257451060256615,
-5.21917748504818));
#29982=CARTESIAN_POINT('Ctrl Pts',(-0.276554039340992,0.0461724880261877,
-5.20329189962367));
#29983=CARTESIAN_POINT('Ctrl Pts',(-0.188665699985335,-0.207410918168237,
-5.18740631419917));
#29984=CARTESIAN_POINT('Ctrl Pts',(0.0720846932421861,-0.270957251843399,
-5.17152072877465));
#29985=CARTESIAN_POINT('Ctrl Pts',(0.266788591915922,-0.0862431594381096,
-5.15563514335015));
#29986=CARTESIAN_POINT('Ctrl Pts',(0.217051535229177,0.177489905011538,
-5.13974955792564));
#29987=CARTESIAN_POINT('Ctrl Pts',(-0.0315556614918893,0.278600566320595,
-5.12386397250114));
#29988=CARTESIAN_POINT('Ctrl Pts',(-0.251250467369271,0.124447731892029,
-5.10797838707663));
#29989=CARTESIAN_POINT('Ctrl Pts',(-0.240740886179508,-0.143728428113065,
-5.09209280165212));
#29990=CARTESIAN_POINT('Ctrl Pts',(-0.00965616049258788,-0.280215620354914,
-5.07620721622762));
#29991=CARTESIAN_POINT('Ctrl Pts',(0.230275874140234,-0.159959548371763,
-5.0603216308031));
#29992=CARTESIAN_POINT('Ctrl Pts',(0.25922117104535,0.106857006360016,-5.04443604537861));
#29993=CARTESIAN_POINT('Ctrl Pts',(0.0506590458941416,0.275767467978807,
-5.02855045995409));
#29994=CARTESIAN_POINT('Ctrl Pts',(-0.204318653053104,0.192010216761797,
-5.01266487452959));
#29995=CARTESIAN_POINT('Ctrl Pts',(-0.272092519963909,-0.0676734505255753,
-4.99677928910508));
#29996=CARTESIAN_POINT('Ctrl Pts',(-0.0905657887914961,-0.265352356738962,
-4.98089370368057));
#29997=CARTESIAN_POINT('Ctrl Pts',(0.173940457270164,-0.219906236043896,
-4.96500811825607));
#29998=CARTESIAN_POINT('Ctrl Pts',(0.279076427243118,0.0270256005218002,
-4.94912253283156));
#29999=CARTESIAN_POINT('Ctrl Pts',(0.128512901206904,0.249195645125937,
-4.93323694740706));
#30000=CARTESIAN_POINT('Ctrl Pts',(-0.139798599439343,0.243044002026681,
-4.91735136198254));
#30001=CARTESIAN_POINT('Ctrl Pts',(-0.280021777569238,0.0142070198603066,
-4.90146577655804));
#30002=CARTESIAN_POINT('Ctrl Pts',(-0.163679296953366,-0.227646926346919,
-4.88558019113353));
#30003=CARTESIAN_POINT('Ctrl Pts',(0.102631828995819,-0.260922867919469,
-4.86969460570902));
#30004=CARTESIAN_POINT('Ctrl Pts',(0.274908115786522,-0.0551322337752745,
-4.85380902028452));
#30005=CARTESIAN_POINT('Ctrl Pts',(0.195304058006928,0.201172463951639,
-4.83792343486001));
#30006=CARTESIAN_POINT('Ctrl Pts',(-0.0632443473631996,0.273155977150327,
-4.82203784943551));
#30007=CARTESIAN_POINT('Ctrl Pts',(-0.263846089498633,0.0948645159299668,
-4.806152264011));
#30008=CARTESIAN_POINT('Ctrl Pts',(-0.222702898981555,-0.170345102986727,
-4.79026667858649));
#30009=CARTESIAN_POINT('Ctrl Pts',(0.0224884069277866,-0.279478634031651,
-4.77438109316199));
#30010=CARTESIAN_POINT('Ctrl Pts',(0.247075054914963,-0.13254415326643,
-4.75849550773747));
#30011=CARTESIAN_POINT('Ctrl Pts',(0.245282973454107,0.135831874977338,
-4.74260992231297));
#30012=CARTESIAN_POINT('Ctrl Pts',(0.0187541296969196,0.279754031151758,
-4.72672433688846));
#30013=CARTESIAN_POINT('Ctrl Pts',(-0.224957897745701,0.167355847128752,
-4.71083875146396));
#30014=CARTESIAN_POINT('Ctrl Pts',(-0.262555701765402,-0.0983795649351243,
-4.69495316603945));
#30015=CARTESIAN_POINT('Ctrl Pts',(-0.0595908711013016,-0.273976209565238,
-4.67906758061494));
#30016=CARTESIAN_POINT('Ctrl Pts',(0.197973181209263,-0.198546354406802,
-4.66318199519043));
#30017=CARTESIAN_POINT('Ctrl Pts',(0.274147342733956,0.0587985526884655,
-4.64729640976593));
#30018=CARTESIAN_POINT('Ctrl Pts',(0.0991382063290872,0.262270187730513,
-4.63141082434142));
#30019=CARTESIAN_POINT('Ctrl Pts',(-0.16670479105078,0.225440785944032,
-4.61552523891691));
#30020=CARTESIAN_POINT('Ctrl Pts',(-0.279807080535371,-0.0179452781705858,
-4.59963965349241));
#30021=CARTESIAN_POINT('Ctrl Pts',(-0.13654042413847,-0.244889256404674,
-4.5837540680679));
#30022=CARTESIAN_POINT('Ctrl Pts',(0.131829301628996,-0.247457209550174,
-4.56786848264339));
#30023=CARTESIAN_POINT('Ctrl Pts',(0.279412451766375,-0.0232962899245847,
-4.55198289721889));
#30024=CARTESIAN_POINT('Ctrl Pts',(0.170988228579068,0.222209498027739,
-4.53609731179438));
#30025=CARTESIAN_POINT('Ctrl Pts',(-0.0941013364397791,0.264119241643986,
-4.52021172636988));
#30026=CARTESIAN_POINT('Ctrl Pts',(-0.272971995264593,0.0640337811441318,
-4.50432614094536));
#30027=CARTESIAN_POINT('Ctrl Pts',(-0.201736250251262,-0.194721649183925,
-4.48844055552086));
#30028=CARTESIAN_POINT('Ctrl Pts',(0.0543372398400151,-0.275066355072582,
-4.47255497009635));
#30029=CARTESIAN_POINT('Ctrl Pts',(0.260625067348198,-0.103385732072151,
-4.45666938467185));
#30030=CARTESIAN_POINT('Ctrl Pts',(0.228119174345422,0.163020482217144,
-4.44078379924733));
#30031=CARTESIAN_POINT('Ctrl Pts',(-0.0133974132773538,0.280061680070342,
-4.42489821382283));
#30032=CARTESIAN_POINT('Ctrl Pts',(-0.242638826473229,0.140500659123159,
-4.40901262839833));
#30033=CARTESIAN_POINT('Ctrl Pts',(-0.249566136488284,-0.127791935757538,
-4.39312704297382));
#30034=CARTESIAN_POINT('Ctrl Pts',(-0.0278323017717629,-0.27899712956307,
-4.37724145754931));
#30035=CARTESIAN_POINT('Ctrl Pts',(0.219402452553475,-0.174575482642516,
-4.36135587212481));
#30036=CARTESIAN_POINT('Ctrl Pts',(0.265613074904189,0.0897982726241923,
-4.3454702867003));
#30037=CARTESIAN_POINT('Ctrl Pts',(0.0684597913264363,0.271895737917843,
-4.32958470127579));
#30038=CARTESIAN_POINT('Ctrl Pts',(-0.191418726023258,0.204872903659757,
-4.31369911585128));
#30039=CARTESIAN_POINT('Ctrl Pts',(-0.275912771619538,-0.0498615862520642,
-4.29781353042678));
#30040=CARTESIAN_POINT('Ctrl Pts',(-0.107605972147853,-0.258911162533527,
-4.28192794500227));
#30041=CARTESIAN_POINT('Ctrl Pts',(0.159293148852347,-0.230737357302738,
-4.26604235957777));
#30042=CARTESIAN_POINT('Ctrl Pts',(0.2802423654424,0.00884601252520937,
-4.25015677415325));
#30043=CARTESIAN_POINT('Ctrl Pts',(0.144423813031258,0.240324359056379,
-4.23427118872875));
#30044=CARTESIAN_POINT('Ctrl Pts',(-0.123720842908662,0.251609197678298,
-4.21838560330425));
#30045=CARTESIAN_POINT('Ctrl Pts',(-0.278508174154103,0.0323609680896043,
-4.20250001787973));
#30046=CARTESIAN_POINT('Ctrl Pts',(-0.178116662567355,-0.216537502161203,
-4.18661443245523));
#30047=CARTESIAN_POINT('Ctrl Pts',(0.0854715091573248,-0.267036807292018,
-4.17072884703072));
#30048=CARTESIAN_POINT('Ctrl Pts',(0.270747721571937,-0.0728677335311189,
-4.15484326160622));
#30049=CARTESIAN_POINT('Ctrl Pts',(0.207955486803503,0.188065283438102,
-4.1389576761817));
#30050=CARTESIAN_POINT('Ctrl Pts',(-0.0453727731435854,0.276686368987695,
-4.12307209075721));
#30051=CARTESIAN_POINT('Ctrl Pts',(-0.257128925622131,0.111797812746169,
-4.10718650533269));
#30052=CARTESIAN_POINT('Ctrl Pts',(-0.233294643822228,-0.155523774678048,
-4.09130091990819));
#30053=CARTESIAN_POINT('Ctrl Pts',(0.00429227712398719,-0.280349088964778,
-4.07541533448367));
#30054=CARTESIAN_POINT('Ctrl Pts',(0.237946464991633,-0.148308850460187,
-4.05952974905918));
#30055=CARTESIAN_POINT('Ctrl Pts',(0.253585853911662,0.11961709752968,-4.04364416363466));
#30056=CARTESIAN_POINT('Ctrl Pts',(0.0368810936713182,0.2779457145844,-4.02775857821017));
#30057=CARTESIAN_POINT('Ctrl Pts',(-0.213615402978162,0.1816108337631,-4.01187299278565));
#30058=CARTESIAN_POINT('Ctrl Pts',(-0.268390063041775,-0.0811221879655325,
-3.99598740736115));
#30059=CARTESIAN_POINT('Ctrl Pts',(-0.0772564444343335,-0.269528249207591,
-3.98010182193664));
#30060=CARTESIAN_POINT('Ctrl Pts',(0.184662206520241,-0.210983186133545,
-3.96421623651213));
#30061=CARTESIAN_POINT('Ctrl Pts',(0.277386942916036,0.0408719852250892,
-3.94833065108763));
#30062=CARTESIAN_POINT('Ctrl Pts',(0.115960147730902,0.25527882694822,-3.93244506566312));
#30063=CARTESIAN_POINT('Ctrl Pts',(-0.151713354856548,0.235790359050968,
-3.91655948023861));
#30064=CARTESIAN_POINT('Ctrl Pts',(-0.280381821803572,0.000262590967015663,
-3.9006738948141));
#30065=CARTESIAN_POINT('Ctrl Pts',(-0.152154747356785,-0.235505771598453,
-3.8847883093896));
#30066=CARTESIAN_POINT('Ctrl Pts',(0.115481785178347,-0.255495584003526,
-3.86890272396509));
#30067=CARTESIAN_POINT('Ctrl Pts',(0.277309894480033,-0.0413914846015558,
-3.85301713854059));
#30068=CARTESIAN_POINT('Ctrl Pts',(0.185057083358657,0.210636924353684,
-3.83713155311608));
#30069=CARTESIAN_POINT('Ctrl Pts',(-0.0767514749289204,0.269672488584438,
-3.82124596769156));
#30070=CARTESIAN_POINT('Ctrl Pts',(-0.268237607872236,0.0816247588364526,
-3.80536038226707));
#30071=CARTESIAN_POINT('Ctrl Pts',(-0.213955269833982,-0.181210380025067,
-3.78947479684255));
#30072=CARTESIAN_POINT('Ctrl Pts',(0.0363605403484637,-0.278014334385727,
-3.77358921141805));
#30073=CARTESIAN_POINT('Ctrl Pts',(0.253361103521349,-0.12009182855713,
-3.75770362599354));
#30074=CARTESIAN_POINT('Ctrl Pts',(0.238224329987279,0.147862798361475,
-3.74181804056903));
#30075=CARTESIAN_POINT('Ctrl Pts',(0.00481645089103148,0.280340742181402,
-3.72593245514453));
#30076=CARTESIAN_POINT('Ctrl Pts',(-0.233001108592176,0.155960127531069,
-3.71004686972002));
#30077=CARTESIAN_POINT('Ctrl Pts',(-0.2573413909844,-0.111315299145181,
-3.69416128429552));
#30078=CARTESIAN_POINT('Ctrl Pts',(-0.0458841718383633,-0.276602230999808,
-3.67827569887101));
#30079=CARTESIAN_POINT('Ctrl Pts',(0.207589749925143,-0.188451893574426,
-3.6623901134465));
#30080=CARTESIAN_POINT('Ctrl Pts',(0.27090907321563,0.0723554809013986,
-3.64650452802199));
#30081=CARTESIAN_POINT('Ctrl Pts',(0.0859225438163616,0.266885897640616,
-3.63061894259749));
#30082=CARTESIAN_POINT('Ctrl Pts',(-0.177615800257995,0.216851966830158,
-3.61473335717298));
#30083=CARTESIAN_POINT('Ctrl Pts',(-0.27875419449686,-0.0318017367932098,
-3.59884777174848));
#30084=CARTESIAN_POINT('Ctrl Pts',(-0.123809722470591,-0.251461066226499,
-3.58296218632396));
#30085=CARTESIAN_POINT('Ctrl Pts',(0.0540749562403304,-0.24403817460498,
-3.57237179604096));
#30086=CARTESIAN_POINT('Ctrl Pts',(0.12178706197938,-0.203518775938317,
-3.56707660089946));
#30087=CARTESIAN_POINT('',(0.151068846355364,-0.252451665989471,-3.6));
#30088=CARTESIAN_POINT('Ctrl Pts',(-0.237357402024655,-0.00992348605842327,
-3.6));
#30089=CARTESIAN_POINT('Ctrl Pts',(-0.237818158165497,-0.0156781358441794,
-3.6));
#30090=CARTESIAN_POINT('Ctrl Pts',(-0.238053973041474,-0.0214395997296665,
-3.6));
#30091=CARTESIAN_POINT('Ctrl Pts',(-0.238060167870929,-0.0271962756202516,
-3.6));
#30092=CARTESIAN_POINT('Ctrl Pts',(-0.23807319373073,-0.0393008304937199,
-3.6));
#30093=CARTESIAN_POINT('Ctrl Pts',(-0.237072714474431,-0.0513839386958204,
-3.6));
#30094=CARTESIAN_POINT('Ctrl Pts',(-0.235138076370835,-0.0633587566056082,
-3.6));
#30095=CARTESIAN_POINT('Ctrl Pts',(-0.234045286901415,-0.0701227890547415,
-3.6));
#30096=CARTESIAN_POINT('Ctrl Pts',(-0.232652433897081,-0.0768567577364692,
-3.6));
#30097=CARTESIAN_POINT('Ctrl Pts',(-0.230979008350505,-0.0835169074499154,
-3.6));
#30098=CARTESIAN_POINT('Ctrl Pts',(-0.228489157220848,-0.0934263900209443,
-3.6));
#30099=CARTESIAN_POINT('Ctrl Pts',(-0.225377725547669,-0.103183572699323,
-3.6));
#30100=CARTESIAN_POINT('Ctrl Pts',(-0.22168847500784,-0.112738759405678,
-3.6));
#30101=CARTESIAN_POINT('Ctrl Pts',(-0.219352585423726,-0.118788731035598,
-3.6));
#30102=CARTESIAN_POINT('Ctrl Pts',(-0.216784829686237,-0.124757762683027,
-3.6));
#30103=CARTESIAN_POINT('Ctrl Pts',(-0.213994183376544,-0.130633189689497,
-3.6));
#30104=CARTESIAN_POINT('Ctrl Pts',(-0.21192012642273,-0.134999909397786,
-3.6));
#30105=CARTESIAN_POINT('Ctrl Pts',(-0.209722616116855,-0.139314910937566,
-3.6));
#30106=CARTESIAN_POINT('Ctrl Pts',(-0.207412785002291,-0.143559868692326,
-3.6));
#30107=CARTESIAN_POINT('Ctrl Pts',(-0.199758222129867,-0.157627259082777,
-3.6));
#30108=CARTESIAN_POINT('Ctrl Pts',(-0.190857579307457,-0.170962640513682,
-3.6));
#30109=CARTESIAN_POINT('Ctrl Pts',(-0.18085588350525,-0.18338771537786,
-3.6));
#30110=CARTESIAN_POINT('Ctrl Pts',(-0.173977043171628,-0.19193327683206,
-3.6));
#30111=CARTESIAN_POINT('Ctrl Pts',(-0.166576167133203,-0.200048359000074,
-3.6));
#30112=CARTESIAN_POINT('Ctrl Pts',(-0.158687164513189,-0.207670103762131,
-3.6));
#30113=CARTESIAN_POINT('Ctrl Pts',(-0.154249377376733,-0.211957550793344,
-3.6));
#30114=CARTESIAN_POINT('Ctrl Pts',(-0.149652386008849,-0.216092093447304,
-3.6));
#30115=CARTESIAN_POINT('Ctrl Pts',(-0.14492682489689,-0.220041323919562,
-3.6));
#30116=CARTESIAN_POINT('Ctrl Pts',(-0.136444610605299,-0.227130052296771,
-3.6));
#30117=CARTESIAN_POINT('Ctrl Pts',(-0.127537649227004,-0.233634454227581,
-3.6));
#30118=CARTESIAN_POINT('Ctrl Pts',(-0.118247429613959,-0.239497288460027,
-3.6));
#30119=CARTESIAN_POINT('Ctrl Pts',(-0.108421132217647,-0.245698428492541,
-3.6));
#30120=CARTESIAN_POINT('Ctrl Pts',(-0.0981660718109667,-0.251182303133843,
-3.6));
#30121=CARTESIAN_POINT('Ctrl Pts',(-0.0875605794596233,-0.255961502708628,
-3.6));
#30122=CARTESIAN_POINT('Ctrl Pts',(-0.0808528732519119,-0.25898422580282,
-3.6));
#30123=CARTESIAN_POINT('Ctrl Pts',(-0.0740047561970901,-0.261724835303419,
-3.6));
#30124=CARTESIAN_POINT('Ctrl Pts',(-0.0670343043536097,-0.264184035594139,
-3.6));
#30125=CARTESIAN_POINT('Ctrl Pts',(-0.0628591814074491,-0.265657033872234,
-3.6));
#30126=CARTESIAN_POINT('Ctrl Pts',(-0.0586406755024959,-0.2670286085373,
-3.6));
#30127=CARTESIAN_POINT('Ctrl Pts',(-0.0543960005259033,-0.268295339221923,
-3.6));
#30128=CARTESIAN_POINT('Ctrl Pts',(-0.0385528896482364,-0.273023370178188,
-3.6));
#30129=CARTESIAN_POINT('Ctrl Pts',(-0.0223017363277034,-0.27631099702761,
-3.6));
#30130=CARTESIAN_POINT('Ctrl Pts',(-0.00585688672513749,-0.278193970555172,
-3.6));
#30131=CARTESIAN_POINT('Ctrl Pts',(0.00913418873160995,-0.279910483561794,
-3.6));
#30132=CARTESIAN_POINT('Ctrl Pts',(0.0242875292752077,-0.280459386992588,
-3.6));
#30133=CARTESIAN_POINT('Ctrl Pts',(0.039455058586787,-0.279835389708545,
-3.6));
#30134=CARTESIAN_POINT('Ctrl Pts',(0.0439432239296933,-0.279650745068882,
-3.6));
#30135=CARTESIAN_POINT('Ctrl Pts',(0.0484311331096738,-0.27936305622478,
-3.6));
#30136=CARTESIAN_POINT('Ctrl Pts',(0.0529025262859033,-0.278973505850679,
-3.6));
#30137=CARTESIAN_POINT('Ctrl Pts',(0.0703010175478352,-0.27745773917288,
-3.6));
#30138=CARTESIAN_POINT('Ctrl Pts',(0.0874990268864668,-0.27440207329904,
-3.6));
#30139=CARTESIAN_POINT('Ctrl Pts',(0.104273027409705,-0.269821510755089,
-3.6));
#30140=CARTESIAN_POINT('Ctrl Pts',(0.120323834386248,-0.265438434390266,
-3.6));
#30141=CARTESIAN_POINT('Ctrl Pts',(0.135987913442794,-0.259659004054616,
-3.6));
#30142=CARTESIAN_POINT('Ctrl Pts',(0.151068846355364,-0.252451665989471,
-3.6));
#30143=CARTESIAN_POINT('Ctrl Pts',(0.151068846355364,-0.252451665989471,
-3.6));
#30144=CARTESIAN_POINT('Ctrl Pts',(0.0670764293281557,-0.302713317039253,
-3.6052951951415));
#30145=CARTESIAN_POINT('Ctrl Pts',(-0.043250697217123,-0.307317121645665,
-3.610590390283));
#30146=CARTESIAN_POINT('Ctrl Pts',(-0.130447332883655,-0.264206863645807,
-3.61588558542451));
#30147=CARTESIAN_POINT('Ctrl Pts',(-0.217643968550187,-0.22109660564595,
-3.62118078056601));
#30148=CARTESIAN_POINT('Ctrl Pts',(-0.281710113337973,-0.130272285039823,
-3.62647597570751));
#30149=CARTESIAN_POINT('Ctrl Pts',(-0.292833930551039,-0.033453695162257,
-3.63177117084901));
#30150=CARTESIAN_POINT('Ctrl Pts',(-0.294102228269998,-0.0224147869940842,
-3.63237490999636));
#30151=CARTESIAN_POINT('Ctrl Pts',(-0.294682289386786,-0.0112979548715849,
-3.6329786491437));
#30152=CARTESIAN_POINT('Ctrl Pts',(-0.294602820716591,-0.000172945526623114,
-3.63358238829104));
#30153=CARTESIAN_POINT('Origin',(0.,0.,0.225002200032268));
#30154=CARTESIAN_POINT('',(0.,0.,0.150004400064535));
#30155=CARTESIAN_POINT('',(-0.249992666559108,-3.06152718911923E-17,0.3));
#30156=CARTESIAN_POINT('',(-0.124996333279554,-1.53076359455962E-17,0.225002200032268));
#30157=CARTESIAN_POINT('Origin',(0.,0.,0.3));
#30158=CARTESIAN_POINT('Origin',(0.144337567297406,0.25,0.6));
#30159=CARTESIAN_POINT('',(0.144337567297406,0.25,0.6));
#30160=CARTESIAN_POINT('',(0.288675134594813,0.,0.6));
#30161=CARTESIAN_POINT('',(0.180421959121758,0.1875,0.6));
#30162=CARTESIAN_POINT('',(0.144337567297406,0.25,0.3));
#30163=CARTESIAN_POINT('',(0.144337567297406,0.25,0.6));
#30164=CARTESIAN_POINT('',(0.288675134594813,0.,0.3));
#30165=CARTESIAN_POINT('',(0.288675134594813,0.,0.3));
#30166=CARTESIAN_POINT('',(0.288675134594813,0.,0.6));
#30167=CARTESIAN_POINT('Origin',(-0.144337567297406,0.25,0.6));
#30168=CARTESIAN_POINT('',(-0.144337567297406,0.25,0.6));
#30169=CARTESIAN_POINT('',(-0.0721687836487032,0.25,0.6));
#30170=CARTESIAN_POINT('',(-0.144337567297406,0.25,0.3));
#30171=CARTESIAN_POINT('',(-0.144337567297406,0.25,0.6));
#30172=CARTESIAN_POINT('',(0.144337567297406,0.25,0.3));
#30173=CARTESIAN_POINT('Origin',(-0.288675134594813,5.55111512312578E-17,
0.6));
#30174=CARTESIAN_POINT('',(-0.288675134594813,3.53525079574969E-17,0.6));
#30175=CARTESIAN_POINT('',(-0.252590742770461,0.0625000000000001,0.6));
#30176=CARTESIAN_POINT('',(-0.288675134594813,5.55111512312578E-17,0.3));
#30177=CARTESIAN_POINT('',(-0.288675134594813,3.53525079574969E-17,0.6));
#30178=CARTESIAN_POINT('',(-0.144337567297406,0.25,0.3));
#30179=CARTESIAN_POINT('Origin',(-0.144337567297407,-0.25,0.6));
#30180=CARTESIAN_POINT('',(-0.144337567297407,-0.25,0.6));
#30181=CARTESIAN_POINT('',(-0.180421959121758,-0.1875,0.6));
#30182=CARTESIAN_POINT('',(-0.144337567297407,-0.25,0.3));
#30183=CARTESIAN_POINT('',(-0.144337567297407,-0.25,0.6));
#30184=CARTESIAN_POINT('',(-0.288675134594813,3.53525079574969E-17,0.3));
#30185=CARTESIAN_POINT('Origin',(0.144337567297406,-0.25,0.6));
#30186=CARTESIAN_POINT('',(0.144337567297406,-0.25,0.6));
#30187=CARTESIAN_POINT('',(0.0721687836487032,-0.25,0.6));
#30188=CARTESIAN_POINT('',(0.144337567297406,-0.25,0.3));
#30189=CARTESIAN_POINT('',(0.144337567297406,-0.25,0.6));
#30190=CARTESIAN_POINT('',(-0.144337567297407,-0.25,0.3));
#30191=CARTESIAN_POINT('Origin',(0.288675134594813,0.,0.6));
#30192=CARTESIAN_POINT('',(0.252590742770461,-0.0625,0.6));
#30193=CARTESIAN_POINT('',(0.144337567297406,-0.25,0.3));
#30194=CARTESIAN_POINT('Origin',(0.,0.,0.3));
#30195=CARTESIAN_POINT('Origin',(0.497072620864318,-0.210994809384208,0.56));
#30196=CARTESIAN_POINT('',(0.466514061501753,-0.179901724341759,0.1));
#30197=CARTESIAN_POINT('',(0.466514061501753,-0.179901724341759,0.56));
#30198=CARTESIAN_POINT('',(0.466514061501753,-0.179901724341759,0.29));
#30199=CARTESIAN_POINT('',(0.451052457977236,-0.164169668796321,0.1));
#30200=CARTESIAN_POINT('',(0.497072620864318,-0.210994809384208,0.1));
#30201=CARTESIAN_POINT('',(0.451052457977236,-0.164169668796321,0.56));
#30202=CARTESIAN_POINT('',(0.451052457977236,-0.164169668796321,0.56));
#30203=CARTESIAN_POINT('',(0.497072620864318,-0.210994809384208,0.56));
#30204=CARTESIAN_POINT('Origin',(0.483728513098638,-0.184437764967243,0.56));
#30205=CARTESIAN_POINT('',(0.473009103818409,-0.162056742238344,0.56));
#30206=CARTESIAN_POINT('Origin',(0.,0.,0.56));
#30207=CARTESIAN_POINT('',(0.451052457977236,-0.164169668796321,0.56));
#30208=CARTESIAN_POINT('Origin',(0.451052457977236,-0.164169668796321,0.56));
#30209=CARTESIAN_POINT('',(0.473009103818409,-0.162056742238344,0.1));
#30210=CARTESIAN_POINT('',(0.473009103818409,-0.162056742238344,0.29));
#30211=CARTESIAN_POINT('',(0.451052457977236,-0.164169668796321,0.1));
#30212=CARTESIAN_POINT('Origin',(0.483728513098638,-0.184437764967243,0.1));
#30213=CARTESIAN_POINT('Origin',(0.,0.,0.1));
#30214=CARTESIAN_POINT('Origin',(0.394930998874352,-0.368279114433749,0.56));
#30215=CARTESIAN_POINT('',(0.376849807542158,-0.328609529008881,0.1));
#30216=CARTESIAN_POINT('',(0.376849807542158,-0.328609529008881,0.56));
#30217=CARTESIAN_POINT('',(0.376849807542158,-0.328609529008881,0.29));
#30218=CARTESIAN_POINT('',(0.367701332697109,-0.308538052649539,0.1));
#30219=CARTESIAN_POINT('',(0.394930998874352,-0.368279114433749,0.1));
#30220=CARTESIAN_POINT('',(0.367701332697109,-0.308538052649539,0.56));
#30221=CARTESIAN_POINT('',(0.367701332697109,-0.308538052649539,0.56));
#30222=CARTESIAN_POINT('',(0.394930998874352,-0.368279114433749,0.56));
#30223=CARTESIAN_POINT('Origin',(0.399482254061324,-0.338408583541644,0.56));
#30224=CARTESIAN_POINT('',(0.389056494215466,-0.314062166312295,0.56));
#30225=CARTESIAN_POINT('Origin',(0.,0.,0.56));
#30226=CARTESIAN_POINT('',(0.367701332697109,-0.308538052649539,0.56));
#30227=CARTESIAN_POINT('Origin',(0.367701332697109,-0.308538052649539,0.56));
#30228=CARTESIAN_POINT('',(0.389056494215466,-0.314062166312295,0.1));
#30229=CARTESIAN_POINT('',(0.389056494215466,-0.314062166312295,0.29));
#30230=CARTESIAN_POINT('',(0.367701332697109,-0.308538052649539,0.1));
#30231=CARTESIAN_POINT('Origin',(0.399482254061324,-0.338408583541644,0.1));
#30232=CARTESIAN_POINT('Origin',(0.,0.,0.1));
#30233=CARTESIAN_POINT('Origin',(0.245154869859355,-0.481143523061719,0.56));
#30234=CARTESIAN_POINT('',(0.241731905082157,-0.437682174717398,0.1));
#30235=CARTESIAN_POINT('',(0.241731905082157,-0.437682174717398,0.56));
#30236=CARTESIAN_POINT('',(0.241731905082157,-0.437682174717398,0.29));
#30237=CARTESIAN_POINT('',(0.24,-0.41569219381653,0.1));
#30238=CARTESIAN_POINT('',(0.245154869859355,-0.481143523061719,0.1));
#30239=CARTESIAN_POINT('',(0.24,-0.41569219381653,0.56));
#30240=CARTESIAN_POINT('',(0.24,-0.41569219381653,0.56));
#30241=CARTESIAN_POINT('',(0.245154869859355,-0.481143523061719,0.56));
#30242=CARTESIAN_POINT('Origin',(0.267052539454057,-0.448417858439125,0.56));
#30243=CARTESIAN_POINT('',(0.258177929547807,-0.428187058065056,0.56));
#30244=CARTESIAN_POINT('Origin',(0.,0.,0.56));
#30245=CARTESIAN_POINT('',(0.24,-0.41569219381653,0.56));
#30246=CARTESIAN_POINT('Origin',(0.24,-0.41569219381653,0.56));
#30247=CARTESIAN_POINT('',(0.258177929547807,-0.428187058065056,0.1));
#30248=CARTESIAN_POINT('',(0.258177929547807,-0.428187058065056,0.29));
#30249=CARTESIAN_POINT('',(0.24,-0.41569219381653,0.1));
#30250=CARTESIAN_POINT('Origin',(0.267052539454057,-0.448417858439125,0.1));
#30251=CARTESIAN_POINT('Origin',(0.,0.,0.1));
#30252=CARTESIAN_POINT('Origin',(0.0658094454387798,-0.535974921886314,
0.56));
#30253=CARTESIAN_POINT('',(0.0774575672862877,-0.493963890654054,0.1));
#30254=CARTESIAN_POINT('',(0.0774575672862877,-0.493963890654054,0.56));
#30255=CARTESIAN_POINT('',(0.0774575672862877,-0.493963890654054,0.29));
#30256=CARTESIAN_POINT('',(0.0833511252801264,-0.47270772144586,0.1));
#30257=CARTESIAN_POINT('',(0.0658094454387798,-0.535974921886314,0.1));
#30258=CARTESIAN_POINT('',(0.0833511252801264,-0.47270772144586,0.56));
#30259=CARTESIAN_POINT('',(0.0833511252801264,-0.47270772144586,0.56));
#30260=CARTESIAN_POINT('',(0.0658094454387798,-0.535974921886314,0.56));
#30261=CARTESIAN_POINT('Origin',(0.0936415073922334,-0.504341321666087,
0.56));
#30262=CARTESIAN_POINT('',(0.0961592962762517,-0.490666271247226,0.56));
#30263=CARTESIAN_POINT('Origin',(0.,0.,0.56));
#30264=CARTESIAN_POINT('',(0.0833511252801264,-0.47270772144586,0.56));
#30265=CARTESIAN_POINT('Origin',(0.0833511252801264,-0.47270772144586,0.56));
#30266=CARTESIAN_POINT('',(0.0961592962762517,-0.490666271247226,0.1));
#30267=CARTESIAN_POINT('',(0.0961592962762517,-0.490666271247226,0.29));
#30268=CARTESIAN_POINT('',(0.0833511252801264,-0.47270772144586,0.1));
#30269=CARTESIAN_POINT('Origin',(0.0936415073922334,-0.504341321666087,
0.1));
#30270=CARTESIAN_POINT('Origin',(0.,0.,0.1));
#30271=CARTESIAN_POINT('Origin',(-0.121473569345687,-0.526159834984027,
0.56));
#30272=CARTESIAN_POINT('',(-0.0961592962762519,-0.490666271247226,0.1));
#30273=CARTESIAN_POINT('',(-0.0961592962762519,-0.490666271247226,0.56));
#30274=CARTESIAN_POINT('',(-0.0961592962762519,-0.490666271247226,0.29));
#30275=CARTESIAN_POINT('',(-0.0833511252801266,-0.47270772144586,0.1));
#30276=CARTESIAN_POINT('',(-0.121473569345687,-0.526159834984027,0.1));
#30277=CARTESIAN_POINT('',(-0.0833511252801266,-0.47270772144586,0.56));
#30278=CARTESIAN_POINT('',(-0.0833511252801266,-0.47270772144586,0.56));
#30279=CARTESIAN_POINT('',(-0.121473569345687,-0.526159834984027,0.56));
#30280=CARTESIAN_POINT('Origin',(-0.0936415073922334,-0.504341321666087,
0.56));
#30281=CARTESIAN_POINT('',(-0.0774575672862877,-0.493963890654054,0.56));
#30282=CARTESIAN_POINT('Origin',(0.,0.,0.56));
#30283=CARTESIAN_POINT('',(-0.0833511252801266,-0.47270772144586,0.56));
#30284=CARTESIAN_POINT('Origin',(-0.0833511252801266,-0.47270772144586,
0.56));
#30285=CARTESIAN_POINT('',(-0.0774575672862877,-0.493963890654054,0.1));
#30286=CARTESIAN_POINT('',(-0.0774575672862877,-0.493963890654054,0.29));
#30287=CARTESIAN_POINT('',(-0.0833511252801266,-0.47270772144586,0.1));
#30288=CARTESIAN_POINT('Origin',(-0.0936415073922334,-0.504341321666087,
0.1));
#30289=CARTESIAN_POINT('Origin',(0.,0.,0.1));
#30290=CARTESIAN_POINT('Origin',(-0.294105078908115,-0.452882106690529,
0.56));
#30291=CARTESIAN_POINT('',(-0.258177929547807,-0.428187058065056,0.1));
#30292=CARTESIAN_POINT('',(-0.258177929547807,-0.428187058065056,0.56));
#30293=CARTESIAN_POINT('',(-0.258177929547807,-0.428187058065056,0.29));
#30294=CARTESIAN_POINT('',(-0.24,-0.41569219381653,0.1));
#30295=CARTESIAN_POINT('',(-0.294105078908115,-0.452882106690529,0.1));
#30296=CARTESIAN_POINT('',(-0.24,-0.41569219381653,0.56));
#30297=CARTESIAN_POINT('',(-0.24,-0.41569219381653,0.56));
#30298=CARTESIAN_POINT('',(-0.294105078908115,-0.452882106690529,0.56));
#30299=CARTESIAN_POINT('Origin',(-0.267052539454057,-0.448417858439125,
0.56));
#30300=CARTESIAN_POINT('',(-0.241731905082157,-0.437682174717398,0.56));
#30301=CARTESIAN_POINT('Origin',(0.,0.,0.56));
#30302=CARTESIAN_POINT('',(-0.24,-0.41569219381653,0.56));
#30303=CARTESIAN_POINT('Origin',(-0.24,-0.41569219381653,0.56));
#30304=CARTESIAN_POINT('',(-0.241731905082157,-0.437682174717398,0.1));
#30305=CARTESIAN_POINT('',(-0.241731905082157,-0.437682174717398,0.29));
#30306=CARTESIAN_POINT('',(-0.24,-0.41569219381653,0.1));
#30307=CARTESIAN_POINT('Origin',(-0.267052539454057,-0.448417858439125,
0.1));
#30308=CARTESIAN_POINT('Origin',(0.,0.,0.1));
#30309=CARTESIAN_POINT('Origin',(-0.431263175425538,-0.324980112502106,
0.56));
#30310=CARTESIAN_POINT('',(-0.389056494215466,-0.314062166312295,0.1));
#30311=CARTESIAN_POINT('',(-0.389056494215466,-0.314062166312295,0.56));
#30312=CARTESIAN_POINT('',(-0.389056494215466,-0.314062166312295,0.29));
#30313=CARTESIAN_POINT('',(-0.367701332697109,-0.308538052649539,0.1));
#30314=CARTESIAN_POINT('',(-0.431263175425538,-0.324980112502106,0.1));
#30315=CARTESIAN_POINT('',(-0.367701332697109,-0.308538052649539,0.56));
#30316=CARTESIAN_POINT('',(-0.367701332697109,-0.308538052649539,0.56));
#30317=CARTESIAN_POINT('',(-0.431263175425538,-0.324980112502106,0.56));
#30318=CARTESIAN_POINT('Origin',(-0.399482254061324,-0.338408583541644,
0.56));
#30319=CARTESIAN_POINT('',(-0.376849807542158,-0.328609529008881,0.56));
#30320=CARTESIAN_POINT('Origin',(0.,0.,0.56));
#30321=CARTESIAN_POINT('',(-0.367701332697109,-0.308538052649539,0.56));
#30322=CARTESIAN_POINT('Origin',(-0.367701332697109,-0.308538052649539,
0.56));
#30323=CARTESIAN_POINT('',(-0.376849807542158,-0.328609529008881,0.1));
#30324=CARTESIAN_POINT('',(-0.376849807542158,-0.328609529008881,0.29));
#30325=CARTESIAN_POINT('',(-0.367701332697109,-0.308538052649539,0.1));
#30326=CARTESIAN_POINT('Origin',(-0.399482254061324,-0.338408583541644,
0.1));
#30327=CARTESIAN_POINT('Origin',(0.,0.,0.1));
#30328=CARTESIAN_POINT('Origin',(-0.516404568220039,-0.157880720550278,
0.56));
#30329=CARTESIAN_POINT('',(-0.473009103818409,-0.162056742238344,0.1));
#30330=CARTESIAN_POINT('',(-0.473009103818409,-0.162056742238344,0.56));
#30331=CARTESIAN_POINT('',(-0.473009103818409,-0.162056742238344,0.29));
#30332=CARTESIAN_POINT('',(-0.451052457977236,-0.164169668796321,0.1));
#30333=CARTESIAN_POINT('',(-0.516404568220039,-0.157880720550278,0.1));
#30334=CARTESIAN_POINT('',(-0.451052457977236,-0.164169668796321,0.56));
#30335=CARTESIAN_POINT('',(-0.451052457977236,-0.164169668796321,0.56));
#30336=CARTESIAN_POINT('',(-0.516404568220039,-0.157880720550278,0.56));
#30337=CARTESIAN_POINT('Origin',(-0.483728513098638,-0.184437764967243,
0.56));
#30338=CARTESIAN_POINT('',(-0.466514061501753,-0.179901724341759,0.56));
#30339=CARTESIAN_POINT('Origin',(0.,0.,0.56));
#30340=CARTESIAN_POINT('',(-0.451052457977236,-0.164169668796321,0.56));
#30341=CARTESIAN_POINT('Origin',(-0.451052457977236,-0.164169668796321,
0.56));
#30342=CARTESIAN_POINT('',(-0.466514061501753,-0.179901724341759,0.1));
#30343=CARTESIAN_POINT('',(-0.466514061501753,-0.179901724341759,0.29));
#30344=CARTESIAN_POINT('',(-0.451052457977236,-0.164169668796321,0.1));
#30345=CARTESIAN_POINT('Origin',(-0.483728513098638,-0.184437764967243,
0.1));
#30346=CARTESIAN_POINT('Origin',(0.,0.,0.1));
#30347=CARTESIAN_POINT('Origin',(-0.53925994876747,0.0282614163711897,0.56));
#30348=CARTESIAN_POINT('',(-0.499909834629965,0.00949511665234234,0.1));
#30349=CARTESIAN_POINT('',(-0.499909834629965,0.00949511665234234,0.56));
#30350=CARTESIAN_POINT('',(-0.499909834629965,0.00949511665234234,0.29));
#30351=CARTESIAN_POINT('',(-0.48,5.87830463590729E-17,0.1));
#30352=CARTESIAN_POINT('',(-0.53925994876747,0.0282614163711897,0.1));
#30353=CARTESIAN_POINT('',(-0.48,5.87830463590729E-17,0.56));
#30354=CARTESIAN_POINT('',(-0.48,5.87830463590729E-17,0.56));
#30355=CARTESIAN_POINT('',(-0.53925994876747,0.0282614163711897,0.56));
#30356=CARTESIAN_POINT('Origin',(-0.509629974383735,6.59194920871187E-17,
0.56));
#30357=CARTESIAN_POINT('',(-0.5,-6.12323399573677E-17,0.56));
#30358=CARTESIAN_POINT('Origin',(0.,0.,0.56));
#30359=CARTESIAN_POINT('',(-0.499909834629965,-0.00949511665234226,0.56));
#30360=CARTESIAN_POINT('',(-0.48,5.87830463590729E-17,0.56));
#30361=CARTESIAN_POINT('Origin',(0.,0.,0.56));
#30362=CARTESIAN_POINT('Origin',(-0.48,5.87830463590729E-17,0.56));
#30363=CARTESIAN_POINT('',(-0.499909834629965,-0.00949511665234226,0.1));
#30364=CARTESIAN_POINT('',(-0.499909834629965,-0.00949511665234226,0.29));
#30365=CARTESIAN_POINT('',(-0.48,5.87830463590729E-17,0.1));
#30366=CARTESIAN_POINT('Origin',(-0.509629974383735,6.59194920871187E-17,
0.1));
#30367=CARTESIAN_POINT('',(-0.5,-6.12323399573677E-17,0.1));
#30368=CARTESIAN_POINT('Origin',(0.,0.,0.1));
#30369=CARTESIAN_POINT('Origin',(0.,0.,0.1));
#30370=CARTESIAN_POINT('Origin',(-0.526159834984027,0.121473569345687,0.56));
#30371=CARTESIAN_POINT('',(-0.490666271247226,0.0961592962762519,0.1));
#30372=CARTESIAN_POINT('',(-0.490666271247226,0.0961592962762519,0.56));
#30373=CARTESIAN_POINT('',(-0.490666271247226,0.0961592962762519,0.29));
#30374=CARTESIAN_POINT('',(-0.47270772144586,0.0833511252801265,0.1));
#30375=CARTESIAN_POINT('',(-0.526159834984027,0.121473569345687,0.1));
#30376=CARTESIAN_POINT('',(-0.47270772144586,0.0833511252801265,0.56));
#30377=CARTESIAN_POINT('',(-0.47270772144586,0.0833511252801265,0.56));
#30378=CARTESIAN_POINT('',(-0.526159834984027,0.121473569345687,0.56));
#30379=CARTESIAN_POINT('Origin',(-0.504341321666087,0.0936415073922334,
0.56));
#30380=CARTESIAN_POINT('',(-0.493963890654054,0.0774575672862877,0.56));
#30381=CARTESIAN_POINT('Origin',(0.,0.,0.56));
#30382=CARTESIAN_POINT('',(-0.47270772144586,0.0833511252801265,0.56));
#30383=CARTESIAN_POINT('Origin',(-0.47270772144586,0.0833511252801265,0.56));
#30384=CARTESIAN_POINT('',(-0.493963890654054,0.0774575672862877,0.1));
#30385=CARTESIAN_POINT('',(-0.493963890654054,0.0774575672862877,0.29));
#30386=CARTESIAN_POINT('',(-0.47270772144586,0.0833511252801265,0.1));
#30387=CARTESIAN_POINT('Origin',(-0.504341321666087,0.0936415073922334,
0.1));
#30388=CARTESIAN_POINT('Origin',(0.,0.,0.1));
#30389=CARTESIAN_POINT('Origin',(-0.452882106690529,0.294105078908115,0.56));
#30390=CARTESIAN_POINT('',(-0.428187058065056,0.258177929547807,0.1));
#30391=CARTESIAN_POINT('',(-0.428187058065056,0.258177929547807,0.56));
#30392=CARTESIAN_POINT('',(-0.428187058065056,0.258177929547807,0.29));
#30393=CARTESIAN_POINT('',(-0.415692193816531,0.24,0.1));
#30394=CARTESIAN_POINT('',(-0.452882106690529,0.294105078908115,0.1));
#30395=CARTESIAN_POINT('',(-0.415692193816531,0.24,0.56));
#30396=CARTESIAN_POINT('',(-0.415692193816531,0.24,0.56));
#30397=CARTESIAN_POINT('',(-0.452882106690529,0.294105078908115,0.56));
#30398=CARTESIAN_POINT('Origin',(-0.448417858439125,0.267052539454057,0.56));
#30399=CARTESIAN_POINT('',(-0.437682174717398,0.241731905082157,0.56));
#30400=CARTESIAN_POINT('Origin',(0.,0.,0.56));
#30401=CARTESIAN_POINT('',(-0.415692193816531,0.24,0.56));
#30402=CARTESIAN_POINT('Origin',(-0.415692193816531,0.24,0.56));
#30403=CARTESIAN_POINT('',(-0.437682174717398,0.241731905082157,0.1));
#30404=CARTESIAN_POINT('',(-0.437682174717398,0.241731905082157,0.29));
#30405=CARTESIAN_POINT('',(-0.415692193816531,0.24,0.1));
#30406=CARTESIAN_POINT('Origin',(-0.448417858439125,0.267052539454057,0.1));
#30407=CARTESIAN_POINT('Origin',(0.,0.,0.1));
#30408=CARTESIAN_POINT('Origin',(-0.324980112502106,0.431263175425538,0.56));
#30409=CARTESIAN_POINT('',(-0.314062166312295,0.389056494215465,0.1));
#30410=CARTESIAN_POINT('',(-0.314062166312295,0.389056494215465,0.56));
#30411=CARTESIAN_POINT('',(-0.314062166312295,0.389056494215465,0.29));
#30412=CARTESIAN_POINT('',(-0.308538052649539,0.367701332697109,0.1));
#30413=CARTESIAN_POINT('',(-0.324980112502106,0.431263175425538,0.1));
#30414=CARTESIAN_POINT('',(-0.308538052649539,0.367701332697109,0.56));
#30415=CARTESIAN_POINT('',(-0.308538052649539,0.367701332697109,0.56));
#30416=CARTESIAN_POINT('',(-0.324980112502106,0.431263175425538,0.56));
#30417=CARTESIAN_POINT('Origin',(-0.338408583541644,0.399482254061324,0.56));
#30418=CARTESIAN_POINT('',(-0.328609529008881,0.376849807542158,0.56));
#30419=CARTESIAN_POINT('Origin',(0.,0.,0.56));
#30420=CARTESIAN_POINT('',(-0.308538052649539,0.367701332697109,0.56));
#30421=CARTESIAN_POINT('Origin',(-0.308538052649539,0.367701332697109,0.56));
#30422=CARTESIAN_POINT('',(-0.328609529008881,0.376849807542158,0.1));
#30423=CARTESIAN_POINT('',(-0.328609529008881,0.376849807542158,0.29));
#30424=CARTESIAN_POINT('',(-0.308538052649539,0.367701332697109,0.1));
#30425=CARTESIAN_POINT('Origin',(-0.338408583541644,0.399482254061324,0.1));
#30426=CARTESIAN_POINT('Origin',(0.,0.,0.1));
#30427=CARTESIAN_POINT('Origin',(-0.157880720550278,0.516404568220039,0.56));
#30428=CARTESIAN_POINT('',(-0.162056742238344,0.473009103818409,0.1));
#30429=CARTESIAN_POINT('',(-0.162056742238344,0.473009103818409,0.56));
#30430=CARTESIAN_POINT('',(-0.162056742238344,0.473009103818409,0.29));
#30431=CARTESIAN_POINT('',(-0.164169668796321,0.451052457977236,0.1));
#30432=CARTESIAN_POINT('',(-0.157880720550278,0.516404568220039,0.1));
#30433=CARTESIAN_POINT('',(-0.164169668796321,0.451052457977236,0.56));
#30434=CARTESIAN_POINT('',(-0.164169668796321,0.451052457977236,0.56));
#30435=CARTESIAN_POINT('',(-0.157880720550278,0.516404568220039,0.56));
#30436=CARTESIAN_POINT('Origin',(-0.184437764967243,0.483728513098638,0.56));
#30437=CARTESIAN_POINT('',(-0.179901724341759,0.466514061501753,0.56));
#30438=CARTESIAN_POINT('Origin',(0.,0.,0.56));
#30439=CARTESIAN_POINT('',(-0.164169668796321,0.451052457977236,0.56));
#30440=CARTESIAN_POINT('Origin',(-0.164169668796321,0.451052457977236,0.56));
#30441=CARTESIAN_POINT('',(-0.179901724341759,0.466514061501753,0.1));
#30442=CARTESIAN_POINT('',(-0.179901724341759,0.466514061501753,0.29));
#30443=CARTESIAN_POINT('',(-0.164169668796321,0.451052457977236,0.1));
#30444=CARTESIAN_POINT('Origin',(-0.184437764967243,0.483728513098638,0.1));
#30445=CARTESIAN_POINT('Origin',(0.,0.,0.1));
#30446=CARTESIAN_POINT('Origin',(0.0282614163711897,0.53925994876747,0.56));
#30447=CARTESIAN_POINT('',(0.00949511665234237,0.499909834629964,0.1));
#30448=CARTESIAN_POINT('',(0.00949511665234237,0.499909834629964,0.56));
#30449=CARTESIAN_POINT('',(0.00949511665234237,0.499909834629964,0.29));
#30450=CARTESIAN_POINT('',(2.93915231795365E-17,0.48,0.1));
#30451=CARTESIAN_POINT('',(0.0282614163711897,0.53925994876747,0.1));
#30452=CARTESIAN_POINT('',(2.93915231795365E-17,0.48,0.56));
#30453=CARTESIAN_POINT('',(2.93915231795365E-17,0.48,0.56));
#30454=CARTESIAN_POINT('',(0.0282614163711897,0.53925994876747,0.56));
#30455=CARTESIAN_POINT('Origin',(3.46944695195361E-17,0.509629974383735,
0.56));
#30456=CARTESIAN_POINT('',(-0.00949511665234229,0.499909834629964,0.56));
#30457=CARTESIAN_POINT('Origin',(0.,0.,0.56));
#30458=CARTESIAN_POINT('',(2.93915231795365E-17,0.48,0.56));
#30459=CARTESIAN_POINT('Origin',(2.93915231795365E-17,0.48,0.56));
#30460=CARTESIAN_POINT('',(-0.00949511665234229,0.499909834629964,0.1));
#30461=CARTESIAN_POINT('',(-0.00949511665234229,0.499909834629964,0.29));
#30462=CARTESIAN_POINT('',(2.93915231795365E-17,0.48,0.1));
#30463=CARTESIAN_POINT('Origin',(3.46944695195361E-17,0.509629974383735,
0.1));
#30464=CARTESIAN_POINT('Origin',(0.,0.,0.1));
#30465=CARTESIAN_POINT('Origin',(0.210994809384208,0.497072620864318,0.56));
#30466=CARTESIAN_POINT('',(0.179901724341759,0.466514061501753,0.1));
#30467=CARTESIAN_POINT('',(0.179901724341759,0.466514061501753,0.56));
#30468=CARTESIAN_POINT('',(0.179901724341759,0.466514061501753,0.29));
#30469=CARTESIAN_POINT('',(0.164169668796321,0.451052457977236,0.1));
#30470=CARTESIAN_POINT('',(0.210994809384208,0.497072620864318,0.1));
#30471=CARTESIAN_POINT('',(0.164169668796321,0.451052457977236,0.56));
#30472=CARTESIAN_POINT('',(0.164169668796321,0.451052457977236,0.56));
#30473=CARTESIAN_POINT('',(0.210994809384208,0.497072620864318,0.56));
#30474=CARTESIAN_POINT('Origin',(0.184437764967243,0.483728513098638,0.56));
#30475=CARTESIAN_POINT('',(0.162056742238344,0.473009103818409,0.56));
#30476=CARTESIAN_POINT('Origin',(0.,0.,0.56));
#30477=CARTESIAN_POINT('',(0.164169668796321,0.451052457977236,0.56));
#30478=CARTESIAN_POINT('Origin',(0.164169668796321,0.451052457977236,0.56));
#30479=CARTESIAN_POINT('',(0.162056742238344,0.473009103818409,0.1));
#30480=CARTESIAN_POINT('',(0.162056742238344,0.473009103818409,0.29));
#30481=CARTESIAN_POINT('',(0.164169668796321,0.451052457977236,0.1));
#30482=CARTESIAN_POINT('Origin',(0.184437764967243,0.483728513098638,0.1));
#30483=CARTESIAN_POINT('Origin',(0.,0.,0.1));
#30484=CARTESIAN_POINT('Origin',(0.368279114433749,0.394930998874352,0.56));
#30485=CARTESIAN_POINT('',(0.328609529008881,0.376849807542157,0.1));
#30486=CARTESIAN_POINT('',(0.328609529008881,0.376849807542157,0.56));
#30487=CARTESIAN_POINT('',(0.328609529008881,0.376849807542157,0.29));
#30488=CARTESIAN_POINT('',(0.308538052649539,0.367701332697109,0.1));
#30489=CARTESIAN_POINT('',(0.368279114433749,0.394930998874352,0.1));
#30490=CARTESIAN_POINT('',(0.308538052649539,0.367701332697109,0.56));
#30491=CARTESIAN_POINT('',(0.308538052649539,0.367701332697109,0.56));
#30492=CARTESIAN_POINT('',(0.368279114433749,0.394930998874352,0.56));
#30493=CARTESIAN_POINT('Origin',(0.338408583541644,0.399482254061324,0.56));
#30494=CARTESIAN_POINT('',(0.314062166312295,0.389056494215466,0.56));
#30495=CARTESIAN_POINT('Origin',(0.,0.,0.56));
#30496=CARTESIAN_POINT('',(0.308538052649539,0.367701332697109,0.56));
#30497=CARTESIAN_POINT('Origin',(0.308538052649539,0.367701332697109,0.56));
#30498=CARTESIAN_POINT('',(0.314062166312295,0.389056494215466,0.1));
#30499=CARTESIAN_POINT('',(0.314062166312295,0.389056494215466,0.29));
#30500=CARTESIAN_POINT('',(0.308538052649539,0.367701332697109,0.1));
#30501=CARTESIAN_POINT('Origin',(0.338408583541644,0.399482254061324,0.1));
#30502=CARTESIAN_POINT('Origin',(0.,0.,0.1));
#30503=CARTESIAN_POINT('Origin',(0.481143523061719,0.245154869859355,0.56));
#30504=CARTESIAN_POINT('',(0.437682174717398,0.241731905082157,0.1));
#30505=CARTESIAN_POINT('',(0.437682174717398,0.241731905082157,0.56));
#30506=CARTESIAN_POINT('',(0.437682174717398,0.241731905082157,0.29));
#30507=CARTESIAN_POINT('',(0.415692193816531,0.24,0.1));
#30508=CARTESIAN_POINT('',(0.481143523061719,0.245154869859355,0.1));
#30509=CARTESIAN_POINT('',(0.415692193816531,0.24,0.56));
#30510=CARTESIAN_POINT('',(0.415692193816531,0.24,0.56));
#30511=CARTESIAN_POINT('',(0.481143523061719,0.245154869859355,0.56));
#30512=CARTESIAN_POINT('Origin',(0.448417858439125,0.267052539454057,0.56));
#30513=CARTESIAN_POINT('',(0.428187058065056,0.258177929547807,0.56));
#30514=CARTESIAN_POINT('Origin',(0.,0.,0.56));
#30515=CARTESIAN_POINT('',(0.415692193816531,0.24,0.56));
#30516=CARTESIAN_POINT('Origin',(0.415692193816531,0.24,0.56));
#30517=CARTESIAN_POINT('',(0.428187058065056,0.258177929547807,0.1));
#30518=CARTESIAN_POINT('',(0.428187058065056,0.258177929547807,0.29));
#30519=CARTESIAN_POINT('',(0.415692193816531,0.24,0.1));
#30520=CARTESIAN_POINT('Origin',(0.448417858439125,0.267052539454057,0.1));
#30521=CARTESIAN_POINT('Origin',(0.,0.,0.1));
#30522=CARTESIAN_POINT('Origin',(0.535974921886314,0.0658094454387796,0.56));
#30523=CARTESIAN_POINT('',(0.493963890654054,0.0774575672862878,0.1));
#30524=CARTESIAN_POINT('',(0.493963890654054,0.0774575672862878,0.56));
#30525=CARTESIAN_POINT('',(0.493963890654054,0.0774575672862878,0.29));
#30526=CARTESIAN_POINT('',(0.47270772144586,0.0833511252801266,0.1));
#30527=CARTESIAN_POINT('',(0.535974921886314,0.0658094454387796,0.1));
#30528=CARTESIAN_POINT('',(0.47270772144586,0.0833511252801266,0.56));
#30529=CARTESIAN_POINT('',(0.47270772144586,0.0833511252801266,0.56));
#30530=CARTESIAN_POINT('',(0.535974921886314,0.0658094454387796,0.56));
#30531=CARTESIAN_POINT('Origin',(0.504341321666087,0.0936415073922334,0.56));
#30532=CARTESIAN_POINT('',(0.490666271247226,0.0961592962762519,0.56));
#30533=CARTESIAN_POINT('Origin',(0.,0.,0.56));
#30534=CARTESIAN_POINT('',(0.47270772144586,0.0833511252801266,0.56));
#30535=CARTESIAN_POINT('Origin',(0.47270772144586,0.0833511252801266,0.56));
#30536=CARTESIAN_POINT('',(0.490666271247226,0.0961592962762519,0.1));
#30537=CARTESIAN_POINT('',(0.490666271247226,0.0961592962762519,0.29));
#30538=CARTESIAN_POINT('',(0.47270772144586,0.0833511252801266,0.1));
#30539=CARTESIAN_POINT('Origin',(0.504341321666087,0.0936415073922334,0.1));
#30540=CARTESIAN_POINT('Origin',(0.,0.,0.1));
#30541=CARTESIAN_POINT('Origin',(0.516404568220039,0.157880720550278,0.56));
#30542=CARTESIAN_POINT('',(0.473009103818409,0.162056742238344,0.1));
#30543=CARTESIAN_POINT('',(0.473009103818409,0.162056742238344,0.56));
#30544=CARTESIAN_POINT('',(0.473009103818409,0.162056742238344,0.29));
#30545=CARTESIAN_POINT('',(0.451052457977236,0.164169668796321,0.1));
#30546=CARTESIAN_POINT('',(0.516404568220039,0.157880720550278,0.1));
#30547=CARTESIAN_POINT('',(0.451052457977236,0.164169668796321,0.56));
#30548=CARTESIAN_POINT('',(0.451052457977236,0.164169668796321,0.56));
#30549=CARTESIAN_POINT('',(0.516404568220039,0.157880720550278,0.56));
#30550=CARTESIAN_POINT('Origin',(0.483728513098638,0.184437764967243,0.56));
#30551=CARTESIAN_POINT('',(0.466514061501753,0.179901724341759,0.56));
#30552=CARTESIAN_POINT('Origin',(0.,0.,0.56));
#30553=CARTESIAN_POINT('',(0.451052457977236,0.164169668796321,0.56));
#30554=CARTESIAN_POINT('Origin',(0.451052457977236,0.164169668796321,0.56));
#30555=CARTESIAN_POINT('',(0.466514061501753,0.179901724341759,0.1));
#30556=CARTESIAN_POINT('',(0.466514061501753,0.179901724341759,0.29));
#30557=CARTESIAN_POINT('',(0.451052457977236,0.164169668796321,0.1));
#30558=CARTESIAN_POINT('Origin',(0.483728513098638,0.184437764967243,0.1));
#30559=CARTESIAN_POINT('Origin',(0.,0.,0.1));
#30560=CARTESIAN_POINT('Origin',(0.431263175425538,0.324980112502106,0.56));
#30561=CARTESIAN_POINT('',(0.389056494215466,0.314062166312295,0.1));
#30562=CARTESIAN_POINT('',(0.389056494215466,0.314062166312295,0.56));
#30563=CARTESIAN_POINT('',(0.389056494215466,0.314062166312295,0.29));
#30564=CARTESIAN_POINT('',(0.367701332697109,0.308538052649539,0.1));
#30565=CARTESIAN_POINT('',(0.431263175425538,0.324980112502106,0.1));
#30566=CARTESIAN_POINT('',(0.367701332697109,0.308538052649539,0.56));
#30567=CARTESIAN_POINT('',(0.367701332697109,0.308538052649539,0.56));
#30568=CARTESIAN_POINT('',(0.431263175425538,0.324980112502106,0.56));
#30569=CARTESIAN_POINT('Origin',(0.399482254061324,0.338408583541644,0.56));
#30570=CARTESIAN_POINT('',(0.376849807542158,0.328609529008881,0.56));
#30571=CARTESIAN_POINT('Origin',(0.,0.,0.56));
#30572=CARTESIAN_POINT('',(0.367701332697109,0.308538052649539,0.56));
#30573=CARTESIAN_POINT('Origin',(0.367701332697109,0.308538052649539,0.56));
#30574=CARTESIAN_POINT('',(0.376849807542158,0.328609529008881,0.1));
#30575=CARTESIAN_POINT('',(0.376849807542158,0.328609529008881,0.29));
#30576=CARTESIAN_POINT('',(0.367701332697109,0.308538052649539,0.1));
#30577=CARTESIAN_POINT('Origin',(0.399482254061324,0.338408583541644,0.1));
#30578=CARTESIAN_POINT('Origin',(0.,0.,0.1));
#30579=CARTESIAN_POINT('Origin',(0.294105078908115,0.452882106690529,0.56));
#30580=CARTESIAN_POINT('',(0.258177929547807,0.428187058065056,0.1));
#30581=CARTESIAN_POINT('',(0.258177929547807,0.428187058065056,0.56));
#30582=CARTESIAN_POINT('',(0.258177929547807,0.428187058065056,0.29));
#30583=CARTESIAN_POINT('',(0.24,0.41569219381653,0.1));
#30584=CARTESIAN_POINT('',(0.294105078908115,0.452882106690529,0.1));
#30585=CARTESIAN_POINT('',(0.24,0.41569219381653,0.56));
#30586=CARTESIAN_POINT('',(0.24,0.41569219381653,0.56));
#30587=CARTESIAN_POINT('',(0.294105078908115,0.452882106690529,0.56));
#30588=CARTESIAN_POINT('Origin',(0.267052539454057,0.448417858439125,0.56));
#30589=CARTESIAN_POINT('',(0.241731905082157,0.437682174717398,0.56));
#30590=CARTESIAN_POINT('Origin',(0.,0.,0.56));
#30591=CARTESIAN_POINT('',(0.24,0.41569219381653,0.56));
#30592=CARTESIAN_POINT('Origin',(0.24,0.41569219381653,0.56));
#30593=CARTESIAN_POINT('',(0.241731905082157,0.437682174717398,0.1));
#30594=CARTESIAN_POINT('',(0.241731905082157,0.437682174717398,0.29));
#30595=CARTESIAN_POINT('',(0.24,0.41569219381653,0.1));
#30596=CARTESIAN_POINT('Origin',(0.267052539454057,0.448417858439125,0.1));
#30597=CARTESIAN_POINT('Origin',(0.,0.,0.1));
#30598=CARTESIAN_POINT('Origin',(0.121473569345687,0.526159834984027,0.56));
#30599=CARTESIAN_POINT('',(0.0961592962762519,0.490666271247226,0.1));
#30600=CARTESIAN_POINT('',(0.0961592962762519,0.490666271247226,0.56));
#30601=CARTESIAN_POINT('',(0.0961592962762519,0.490666271247226,0.29));
#30602=CARTESIAN_POINT('',(0.0833511252801266,0.47270772144586,0.1));
#30603=CARTESIAN_POINT('',(0.121473569345687,0.526159834984027,0.1));
#30604=CARTESIAN_POINT('',(0.0833511252801266,0.47270772144586,0.56));
#30605=CARTESIAN_POINT('',(0.0833511252801266,0.47270772144586,0.56));
#30606=CARTESIAN_POINT('',(0.121473569345687,0.526159834984027,0.56));
#30607=CARTESIAN_POINT('Origin',(0.0936415073922334,0.504341321666087,0.56));
#30608=CARTESIAN_POINT('',(0.0774575672862878,0.493963890654054,0.56));
#30609=CARTESIAN_POINT('Origin',(0.,0.,0.56));
#30610=CARTESIAN_POINT('',(0.0833511252801266,0.47270772144586,0.56));
#30611=CARTESIAN_POINT('Origin',(0.0833511252801266,0.47270772144586,0.56));
#30612=CARTESIAN_POINT('',(0.0774575672862878,0.493963890654054,0.1));
#30613=CARTESIAN_POINT('',(0.0774575672862878,0.493963890654054,0.29));
#30614=CARTESIAN_POINT('',(0.0833511252801266,0.47270772144586,0.1));
#30615=CARTESIAN_POINT('Origin',(0.0936415073922334,0.504341321666087,0.1));
#30616=CARTESIAN_POINT('Origin',(0.,0.,0.1));
#30617=CARTESIAN_POINT('Origin',(-0.0658094454387796,0.535974921886314,
0.56));
#30618=CARTESIAN_POINT('',(-0.0774575672862878,0.493963890654054,0.1));
#30619=CARTESIAN_POINT('',(-0.0774575672862878,0.493963890654054,0.56));
#30620=CARTESIAN_POINT('',(-0.0774575672862878,0.493963890654054,0.29));
#30621=CARTESIAN_POINT('',(-0.0833511252801265,0.47270772144586,0.1));
#30622=CARTESIAN_POINT('',(-0.0658094454387796,0.535974921886314,0.1));
#30623=CARTESIAN_POINT('',(-0.0833511252801265,0.47270772144586,0.56));
#30624=CARTESIAN_POINT('',(-0.0833511252801265,0.47270772144586,0.56));
#30625=CARTESIAN_POINT('',(-0.0658094454387796,0.535974921886314,0.56));
#30626=CARTESIAN_POINT('Origin',(-0.0936415073922333,0.504341321666087,
0.56));
#30627=CARTESIAN_POINT('',(-0.0961592962762518,0.490666271247226,0.56));
#30628=CARTESIAN_POINT('Origin',(0.,0.,0.56));
#30629=CARTESIAN_POINT('',(-0.0833511252801265,0.47270772144586,0.56));
#30630=CARTESIAN_POINT('Origin',(-0.0833511252801265,0.47270772144586,0.56));
#30631=CARTESIAN_POINT('',(-0.0961592962762518,0.490666271247226,0.1));
#30632=CARTESIAN_POINT('',(-0.0961592962762518,0.490666271247226,0.29));
#30633=CARTESIAN_POINT('',(-0.0833511252801265,0.47270772144586,0.1));
#30634=CARTESIAN_POINT('Origin',(-0.0936415073922333,0.504341321666087,
0.1));
#30635=CARTESIAN_POINT('Origin',(0.,0.,0.1));
#30636=CARTESIAN_POINT('Origin',(-0.245154869859355,0.481143523061719,0.56));
#30637=CARTESIAN_POINT('',(-0.241731905082157,0.437682174717398,0.1));
#30638=CARTESIAN_POINT('',(-0.241731905082157,0.437682174717398,0.56));
#30639=CARTESIAN_POINT('',(-0.241731905082157,0.437682174717398,0.29));
#30640=CARTESIAN_POINT('',(-0.24,0.415692193816531,0.1));
#30641=CARTESIAN_POINT('',(-0.245154869859355,0.481143523061719,0.1));
#30642=CARTESIAN_POINT('',(-0.24,0.415692193816531,0.56));
#30643=CARTESIAN_POINT('',(-0.24,0.415692193816531,0.56));
#30644=CARTESIAN_POINT('',(-0.245154869859355,0.481143523061719,0.56));
#30645=CARTESIAN_POINT('Origin',(-0.267052539454057,0.448417858439125,0.56));
#30646=CARTESIAN_POINT('',(-0.258177929547807,0.428187058065056,0.56));
#30647=CARTESIAN_POINT('Origin',(0.,0.,0.56));
#30648=CARTESIAN_POINT('',(-0.24,0.415692193816531,0.56));
#30649=CARTESIAN_POINT('Origin',(-0.24,0.415692193816531,0.56));
#30650=CARTESIAN_POINT('',(-0.258177929547807,0.428187058065056,0.1));
#30651=CARTESIAN_POINT('',(-0.258177929547807,0.428187058065056,0.29));
#30652=CARTESIAN_POINT('',(-0.24,0.415692193816531,0.1));
#30653=CARTESIAN_POINT('Origin',(-0.267052539454057,0.448417858439125,0.1));
#30654=CARTESIAN_POINT('Origin',(0.,0.,0.1));
#30655=CARTESIAN_POINT('Origin',(-0.394930998874352,0.368279114433749,0.56));
#30656=CARTESIAN_POINT('',(-0.376849807542157,0.328609529008881,0.1));
#30657=CARTESIAN_POINT('',(-0.376849807542157,0.328609529008881,0.56));
#30658=CARTESIAN_POINT('',(-0.376849807542157,0.328609529008881,0.29));
#30659=CARTESIAN_POINT('',(-0.367701332697109,0.308538052649539,0.1));
#30660=CARTESIAN_POINT('',(-0.394930998874352,0.368279114433749,0.1));
#30661=CARTESIAN_POINT('',(-0.367701332697109,0.308538052649539,0.56));
#30662=CARTESIAN_POINT('',(-0.367701332697109,0.308538052649539,0.56));
#30663=CARTESIAN_POINT('',(-0.394930998874352,0.368279114433749,0.56));
#30664=CARTESIAN_POINT('Origin',(-0.399482254061324,0.338408583541644,0.56));
#30665=CARTESIAN_POINT('',(-0.389056494215466,0.314062166312295,0.56));
#30666=CARTESIAN_POINT('Origin',(0.,0.,0.56));
#30667=CARTESIAN_POINT('',(-0.367701332697109,0.308538052649539,0.56));
#30668=CARTESIAN_POINT('Origin',(-0.367701332697109,0.308538052649539,0.56));
#30669=CARTESIAN_POINT('',(-0.389056494215466,0.314062166312295,0.1));
#30670=CARTESIAN_POINT('',(-0.389056494215466,0.314062166312295,0.29));
#30671=CARTESIAN_POINT('',(-0.367701332697109,0.308538052649539,0.1));
#30672=CARTESIAN_POINT('Origin',(-0.399482254061324,0.338408583541644,0.1));
#30673=CARTESIAN_POINT('Origin',(0.,0.,0.1));
#30674=CARTESIAN_POINT('Origin',(-0.497072620864318,0.210994809384208,0.56));
#30675=CARTESIAN_POINT('',(-0.466514061501753,0.179901724341759,0.1));
#30676=CARTESIAN_POINT('',(-0.466514061501753,0.179901724341759,0.56));
#30677=CARTESIAN_POINT('',(-0.466514061501753,0.179901724341759,0.29));
#30678=CARTESIAN_POINT('',(-0.451052457977236,0.164169668796321,0.1));
#30679=CARTESIAN_POINT('',(-0.497072620864318,0.210994809384208,0.1));
#30680=CARTESIAN_POINT('',(-0.451052457977236,0.164169668796321,0.56));
#30681=CARTESIAN_POINT('',(-0.451052457977236,0.164169668796321,0.56));
#30682=CARTESIAN_POINT('',(-0.497072620864318,0.210994809384208,0.56));
#30683=CARTESIAN_POINT('Origin',(-0.483728513098638,0.184437764967243,0.56));
#30684=CARTESIAN_POINT('',(-0.473009103818409,0.162056742238344,0.56));
#30685=CARTESIAN_POINT('Origin',(0.,0.,0.56));
#30686=CARTESIAN_POINT('',(-0.451052457977236,0.164169668796321,0.56));
#30687=CARTESIAN_POINT('Origin',(-0.451052457977236,0.164169668796321,0.56));
#30688=CARTESIAN_POINT('',(-0.473009103818409,0.162056742238344,0.1));
#30689=CARTESIAN_POINT('',(-0.473009103818409,0.162056742238344,0.29));
#30690=CARTESIAN_POINT('',(-0.451052457977236,0.164169668796321,0.1));
#30691=CARTESIAN_POINT('Origin',(-0.483728513098638,0.184437764967243,0.1));
#30692=CARTESIAN_POINT('Origin',(0.,0.,0.1));
#30693=CARTESIAN_POINT('Origin',(0.509629974383735,0.,0.56));
#30694=CARTESIAN_POINT('',(0.499909834629964,-0.00949511665234232,0.56));
#30695=CARTESIAN_POINT('',(0.499909834629965,0.00949511665234234,0.56));
#30696=CARTESIAN_POINT('Origin',(0.,0.,0.56));
#30697=CARTESIAN_POINT('',(0.48,0.,0.56));
#30698=CARTESIAN_POINT('',(0.53925994876747,-0.0282614163711897,0.56));
#30699=CARTESIAN_POINT('',(0.48,0.,0.56));
#30700=CARTESIAN_POINT('Origin',(0.53925994876747,-0.0282614163711897,0.56));
#30701=CARTESIAN_POINT('',(0.499909834629964,-0.00949511665234232,0.1));
#30702=CARTESIAN_POINT('',(0.499909834629964,-0.00949511665234232,0.29));
#30703=CARTESIAN_POINT('',(0.48,0.,0.1));
#30704=CARTESIAN_POINT('',(0.53925994876747,-0.0282614163711897,0.1));
#30705=CARTESIAN_POINT('',(0.48,0.,0.56));
#30706=CARTESIAN_POINT('Origin',(0.48,0.,0.56));
#30707=CARTESIAN_POINT('',(0.499909834629965,0.00949511665234234,0.1));
#30708=CARTESIAN_POINT('',(0.499909834629965,0.00949511665234234,0.29));
#30709=CARTESIAN_POINT('',(0.48,0.,0.1));
#30710=CARTESIAN_POINT('Origin',(0.509629974383735,0.,0.1));
#30711=CARTESIAN_POINT('Origin',(0.,0.,0.1));
#30712=CARTESIAN_POINT('Origin',(-0.535974921886314,-0.0658094454387796,
0.56));
#30713=CARTESIAN_POINT('',(-0.493963890654054,-0.0774575672862878,0.1));
#30714=CARTESIAN_POINT('',(-0.493963890654054,-0.0774575672862878,0.56));
#30715=CARTESIAN_POINT('',(-0.493963890654054,-0.0774575672862878,0.29));
#30716=CARTESIAN_POINT('',(-0.47270772144586,-0.0833511252801266,0.1));
#30717=CARTESIAN_POINT('',(-0.535974921886314,-0.0658094454387796,0.1));
#30718=CARTESIAN_POINT('',(-0.47270772144586,-0.0833511252801266,0.56));
#30719=CARTESIAN_POINT('',(-0.47270772144586,-0.0833511252801266,0.56));
#30720=CARTESIAN_POINT('',(-0.535974921886314,-0.0658094454387796,0.56));
#30721=CARTESIAN_POINT('Origin',(-0.504341321666087,-0.0936415073922333,
0.56));
#30722=CARTESIAN_POINT('',(-0.490666271247226,-0.0961592962762519,0.56));
#30723=CARTESIAN_POINT('Origin',(0.,0.,0.56));
#30724=CARTESIAN_POINT('',(-0.47270772144586,-0.0833511252801266,0.56));
#30725=CARTESIAN_POINT('Origin',(-0.47270772144586,-0.0833511252801266,
0.56));
#30726=CARTESIAN_POINT('',(-0.490666271247226,-0.0961592962762519,0.1));
#30727=CARTESIAN_POINT('',(-0.490666271247226,-0.0961592962762519,0.29));
#30728=CARTESIAN_POINT('',(-0.47270772144586,-0.0833511252801266,0.1));
#30729=CARTESIAN_POINT('Origin',(-0.504341321666087,-0.0936415073922333,
0.1));
#30730=CARTESIAN_POINT('Origin',(0.,0.,0.1));
#30731=CARTESIAN_POINT('Origin',(-0.481143523061719,-0.245154869859355,
0.56));
#30732=CARTESIAN_POINT('',(-0.437682174717398,-0.241731905082157,0.1));
#30733=CARTESIAN_POINT('',(-0.437682174717398,-0.241731905082157,0.56));
#30734=CARTESIAN_POINT('',(-0.437682174717398,-0.241731905082157,0.29));
#30735=CARTESIAN_POINT('',(-0.41569219381653,-0.24,0.1));
#30736=CARTESIAN_POINT('',(-0.481143523061719,-0.245154869859355,0.1));
#30737=CARTESIAN_POINT('',(-0.41569219381653,-0.24,0.56));
#30738=CARTESIAN_POINT('',(-0.41569219381653,-0.24,0.56));
#30739=CARTESIAN_POINT('',(-0.481143523061719,-0.245154869859355,0.56));
#30740=CARTESIAN_POINT('Origin',(-0.448417858439125,-0.267052539454057,
0.56));
#30741=CARTESIAN_POINT('',(-0.428187058065056,-0.258177929547807,0.56));
#30742=CARTESIAN_POINT('Origin',(0.,0.,0.56));
#30743=CARTESIAN_POINT('',(-0.41569219381653,-0.24,0.56));
#30744=CARTESIAN_POINT('Origin',(-0.41569219381653,-0.24,0.56));
#30745=CARTESIAN_POINT('',(-0.428187058065056,-0.258177929547807,0.1));
#30746=CARTESIAN_POINT('',(-0.428187058065056,-0.258177929547807,0.29));
#30747=CARTESIAN_POINT('',(-0.41569219381653,-0.24,0.1));
#30748=CARTESIAN_POINT('Origin',(-0.448417858439125,-0.267052539454057,
0.1));
#30749=CARTESIAN_POINT('Origin',(0.,0.,0.1));
#30750=CARTESIAN_POINT('Origin',(-0.368279114433749,-0.394930998874352,
0.56));
#30751=CARTESIAN_POINT('',(-0.328609529008881,-0.376849807542157,0.1));
#30752=CARTESIAN_POINT('',(-0.328609529008881,-0.376849807542157,0.56));
#30753=CARTESIAN_POINT('',(-0.328609529008881,-0.376849807542157,0.29));
#30754=CARTESIAN_POINT('',(-0.308538052649539,-0.367701332697109,0.1));
#30755=CARTESIAN_POINT('',(-0.368279114433749,-0.394930998874352,0.1));
#30756=CARTESIAN_POINT('',(-0.308538052649539,-0.367701332697109,0.56));
#30757=CARTESIAN_POINT('',(-0.308538052649539,-0.367701332697109,0.56));
#30758=CARTESIAN_POINT('',(-0.368279114433749,-0.394930998874352,0.56));
#30759=CARTESIAN_POINT('Origin',(-0.338408583541644,-0.399482254061324,
0.56));
#30760=CARTESIAN_POINT('',(-0.314062166312295,-0.389056494215465,0.56));
#30761=CARTESIAN_POINT('Origin',(0.,0.,0.56));
#30762=CARTESIAN_POINT('',(-0.308538052649539,-0.367701332697109,0.56));
#30763=CARTESIAN_POINT('Origin',(-0.308538052649539,-0.367701332697109,
0.56));
#30764=CARTESIAN_POINT('',(-0.314062166312295,-0.389056494215465,0.1));
#30765=CARTESIAN_POINT('',(-0.314062166312295,-0.389056494215465,0.29));
#30766=CARTESIAN_POINT('',(-0.308538052649539,-0.367701332697109,0.1));
#30767=CARTESIAN_POINT('Origin',(-0.338408583541644,-0.399482254061324,
0.1));
#30768=CARTESIAN_POINT('Origin',(0.,0.,0.1));
#30769=CARTESIAN_POINT('Origin',(-0.210994809384208,-0.497072620864318,
0.56));
#30770=CARTESIAN_POINT('',(-0.179901724341759,-0.466514061501753,0.1));
#30771=CARTESIAN_POINT('',(-0.179901724341759,-0.466514061501753,0.56));
#30772=CARTESIAN_POINT('',(-0.179901724341759,-0.466514061501753,0.29));
#30773=CARTESIAN_POINT('',(-0.164169668796321,-0.451052457977236,0.1));
#30774=CARTESIAN_POINT('',(-0.210994809384208,-0.497072620864318,0.1));
#30775=CARTESIAN_POINT('',(-0.164169668796321,-0.451052457977236,0.56));
#30776=CARTESIAN_POINT('',(-0.164169668796321,-0.451052457977236,0.56));
#30777=CARTESIAN_POINT('',(-0.210994809384208,-0.497072620864318,0.56));
#30778=CARTESIAN_POINT('Origin',(-0.184437764967243,-0.483728513098638,
0.56));
#30779=CARTESIAN_POINT('',(-0.162056742238344,-0.473009103818409,0.56));
#30780=CARTESIAN_POINT('Origin',(0.,0.,0.56));
#30781=CARTESIAN_POINT('',(-0.164169668796321,-0.451052457977236,0.56));
#30782=CARTESIAN_POINT('Origin',(-0.164169668796321,-0.451052457977236,
0.56));
#30783=CARTESIAN_POINT('',(-0.162056742238344,-0.473009103818409,0.1));
#30784=CARTESIAN_POINT('',(-0.162056742238344,-0.473009103818409,0.29));
#30785=CARTESIAN_POINT('',(-0.164169668796321,-0.451052457977236,0.1));
#30786=CARTESIAN_POINT('Origin',(-0.184437764967243,-0.483728513098638,
0.1));
#30787=CARTESIAN_POINT('Origin',(0.,0.,0.1));
#30788=CARTESIAN_POINT('Origin',(-0.0282614163711899,-0.53925994876747,
0.56));
#30789=CARTESIAN_POINT('',(-0.00949511665234243,-0.499909834629964,0.1));
#30790=CARTESIAN_POINT('',(-0.00949511665234243,-0.499909834629964,0.56));
#30791=CARTESIAN_POINT('',(-0.00949511665234243,-0.499909834629964,0.29));
#30792=CARTESIAN_POINT('',(-8.81745695386094E-17,-0.48,0.1));
#30793=CARTESIAN_POINT('',(-0.0282614163711899,-0.53925994876747,0.1));
#30794=CARTESIAN_POINT('',(-8.81745695386094E-17,-0.48,0.56));
#30795=CARTESIAN_POINT('',(-8.81745695386094E-17,-0.48,0.56));
#30796=CARTESIAN_POINT('',(-0.0282614163711899,-0.53925994876747,0.56));
#30797=CARTESIAN_POINT('Origin',(-9.71445146547012E-17,-0.509629974383735,
0.56));
#30798=CARTESIAN_POINT('',(0.00949511665234229,-0.499909834629964,0.56));
#30799=CARTESIAN_POINT('Origin',(0.,0.,0.56));
#30800=CARTESIAN_POINT('',(-8.81745695386094E-17,-0.48,0.56));
#30801=CARTESIAN_POINT('Origin',(-8.81745695386094E-17,-0.48,0.56));
#30802=CARTESIAN_POINT('',(0.00949511665234229,-0.499909834629964,0.1));
#30803=CARTESIAN_POINT('',(0.00949511665234229,-0.499909834629964,0.29));
#30804=CARTESIAN_POINT('',(-8.81745695386094E-17,-0.48,0.1));
#30805=CARTESIAN_POINT('Origin',(-9.71445146547012E-17,-0.509629974383735,
0.1));
#30806=CARTESIAN_POINT('Origin',(0.,0.,0.1));
#30807=CARTESIAN_POINT('Origin',(0.157880720550278,-0.516404568220039,0.56));
#30808=CARTESIAN_POINT('',(0.162056742238344,-0.473009103818409,0.1));
#30809=CARTESIAN_POINT('',(0.162056742238344,-0.473009103818409,0.56));
#30810=CARTESIAN_POINT('',(0.162056742238344,-0.473009103818409,0.29));
#30811=CARTESIAN_POINT('',(0.164169668796321,-0.451052457977236,0.1));
#30812=CARTESIAN_POINT('',(0.157880720550278,-0.516404568220039,0.1));
#30813=CARTESIAN_POINT('',(0.164169668796321,-0.451052457977236,0.56));
#30814=CARTESIAN_POINT('',(0.164169668796321,-0.451052457977236,0.56));
#30815=CARTESIAN_POINT('',(0.157880720550278,-0.516404568220039,0.56));
#30816=CARTESIAN_POINT('Origin',(0.184437764967243,-0.483728513098638,0.56));
#30817=CARTESIAN_POINT('',(0.179901724341759,-0.466514061501753,0.56));
#30818=CARTESIAN_POINT('Origin',(0.,0.,0.56));
#30819=CARTESIAN_POINT('',(0.164169668796321,-0.451052457977236,0.56));
#30820=CARTESIAN_POINT('Origin',(0.164169668796321,-0.451052457977236,0.56));
#30821=CARTESIAN_POINT('',(0.179901724341759,-0.466514061501753,0.1));
#30822=CARTESIAN_POINT('',(0.179901724341759,-0.466514061501753,0.29));
#30823=CARTESIAN_POINT('',(0.164169668796321,-0.451052457977236,0.1));
#30824=CARTESIAN_POINT('Origin',(0.184437764967243,-0.483728513098638,0.1));
#30825=CARTESIAN_POINT('Origin',(0.,0.,0.1));
#30826=CARTESIAN_POINT('Origin',(0.324980112502106,-0.431263175425538,0.56));
#30827=CARTESIAN_POINT('',(0.314062166312295,-0.389056494215466,0.1));
#30828=CARTESIAN_POINT('',(0.314062166312295,-0.389056494215466,0.56));
#30829=CARTESIAN_POINT('',(0.314062166312295,-0.389056494215466,0.29));
#30830=CARTESIAN_POINT('',(0.308538052649539,-0.367701332697109,0.1));
#30831=CARTESIAN_POINT('',(0.324980112502106,-0.431263175425538,0.1));
#30832=CARTESIAN_POINT('',(0.308538052649539,-0.367701332697109,0.56));
#30833=CARTESIAN_POINT('',(0.308538052649539,-0.367701332697109,0.56));
#30834=CARTESIAN_POINT('',(0.324980112502106,-0.431263175425538,0.56));
#30835=CARTESIAN_POINT('Origin',(0.338408583541644,-0.399482254061324,0.56));
#30836=CARTESIAN_POINT('',(0.328609529008881,-0.376849807542158,0.56));
#30837=CARTESIAN_POINT('Origin',(0.,0.,0.56));
#30838=CARTESIAN_POINT('',(0.308538052649539,-0.367701332697109,0.56));
#30839=CARTESIAN_POINT('Origin',(0.308538052649539,-0.367701332697109,0.56));
#30840=CARTESIAN_POINT('',(0.328609529008881,-0.376849807542158,0.1));
#30841=CARTESIAN_POINT('',(0.328609529008881,-0.376849807542158,0.29));
#30842=CARTESIAN_POINT('',(0.308538052649539,-0.367701332697109,0.1));
#30843=CARTESIAN_POINT('Origin',(0.338408583541644,-0.399482254061324,0.1));
#30844=CARTESIAN_POINT('Origin',(0.,0.,0.1));
#30845=CARTESIAN_POINT('Origin',(0.452882106690529,-0.294105078908115,0.56));
#30846=CARTESIAN_POINT('',(0.428187058065056,-0.258177929547807,0.1));
#30847=CARTESIAN_POINT('',(0.428187058065056,-0.258177929547807,0.56));
#30848=CARTESIAN_POINT('',(0.428187058065056,-0.258177929547807,0.29));
#30849=CARTESIAN_POINT('',(0.41569219381653,-0.24,0.1));
#30850=CARTESIAN_POINT('',(0.452882106690529,-0.294105078908115,0.1));
#30851=CARTESIAN_POINT('',(0.41569219381653,-0.24,0.56));
#30852=CARTESIAN_POINT('',(0.41569219381653,-0.24,0.56));
#30853=CARTESIAN_POINT('',(0.452882106690529,-0.294105078908115,0.56));
#30854=CARTESIAN_POINT('Origin',(0.448417858439125,-0.267052539454057,0.56));
#30855=CARTESIAN_POINT('',(0.437682174717398,-0.241731905082157,0.56));
#30856=CARTESIAN_POINT('Origin',(0.,0.,0.56));
#30857=CARTESIAN_POINT('',(0.41569219381653,-0.24,0.56));
#30858=CARTESIAN_POINT('Origin',(0.41569219381653,-0.24,0.56));
#30859=CARTESIAN_POINT('',(0.437682174717398,-0.241731905082157,0.1));
#30860=CARTESIAN_POINT('',(0.437682174717398,-0.241731905082157,0.29));
#30861=CARTESIAN_POINT('',(0.41569219381653,-0.24,0.1));
#30862=CARTESIAN_POINT('Origin',(0.448417858439125,-0.267052539454057,0.1));
#30863=CARTESIAN_POINT('Origin',(0.,0.,0.1));
#30864=CARTESIAN_POINT('Origin',(0.526159834984027,-0.121473569345687,0.56));
#30865=CARTESIAN_POINT('',(0.490666271247226,-0.096159296276252,0.1));
#30866=CARTESIAN_POINT('',(0.490666271247226,-0.096159296276252,0.56));
#30867=CARTESIAN_POINT('',(0.490666271247226,-0.096159296276252,0.29));
#30868=CARTESIAN_POINT('',(0.47270772144586,-0.0833511252801266,0.1));
#30869=CARTESIAN_POINT('',(0.526159834984027,-0.121473569345687,0.1));
#30870=CARTESIAN_POINT('',(0.47270772144586,-0.0833511252801266,0.56));
#30871=CARTESIAN_POINT('',(0.47270772144586,-0.0833511252801266,0.56));
#30872=CARTESIAN_POINT('',(0.526159834984027,-0.121473569345687,0.56));
#30873=CARTESIAN_POINT('Origin',(0.504341321666087,-0.0936415073922334,
0.56));
#30874=CARTESIAN_POINT('',(0.493963890654054,-0.0774575672862878,0.56));
#30875=CARTESIAN_POINT('Origin',(0.,0.,0.56));
#30876=CARTESIAN_POINT('',(0.47270772144586,-0.0833511252801266,0.56));
#30877=CARTESIAN_POINT('Origin',(0.47270772144586,-0.0833511252801266,0.56));
#30878=CARTESIAN_POINT('',(0.493963890654054,-0.0774575672862878,0.1));
#30879=CARTESIAN_POINT('',(0.493963890654054,-0.0774575672862878,0.29));
#30880=CARTESIAN_POINT('',(0.47270772144586,-0.0833511252801266,0.1));
#30881=CARTESIAN_POINT('Origin',(0.504341321666087,-0.0936415073922334,
0.1));
#30882=CARTESIAN_POINT('Origin',(0.,0.,0.1));
#30883=CARTESIAN_POINT('Origin',(0.,0.,-0.0249999999999999));
#30884=CARTESIAN_POINT('',(-0.298,-3.64944746145911E-17,-0.0249999999999999));
#30885=CARTESIAN_POINT('Origin',(0.,0.,-0.0249999999999999));
#30886=CARTESIAN_POINT('',(-0.323,-3.95560916124595E-17,0.));
#30887=CARTESIAN_POINT('Origin',(-0.323,-3.95560916124595E-17,-0.0249999999999999));
#30888=CARTESIAN_POINT('Origin',(0.,0.,0.));
#30889=CARTESIAN_POINT('Origin',(0.,0.,-1.8));
#30890=CARTESIAN_POINT('',(-0.298,-3.64944746145911E-17,-3.6));
#30891=CARTESIAN_POINT('',(-0.298,-3.64944746145911E-17,-1.8));
#30892=CARTESIAN_POINT('Origin',(0.,0.,-3.6));
#30893=CARTESIAN_POINT('Origin',(0.48,0.,0.));
#30894=CARTESIAN_POINT('',(-0.48,-5.8783046359073E-17,3.46944695195361E-18));
#30895=CARTESIAN_POINT('Origin',(0.,0.,0.));
#30896=CARTESIAN_POINT('Origin',(0.26,0.,-6.));
#30897=CARTESIAN_POINT('',(-0.26,-3.18408167778312E-17,-6.));
#30898=CARTESIAN_POINT('Origin',(0.,0.,-6.));
#30899=CARTESIAN_POINT('Origin',(0.,0.,-5.98));
#30900=CARTESIAN_POINT('',(-0.28,-3.42901103761259E-17,-5.98));
#30901=CARTESIAN_POINT('Origin',(0.,0.,-4.78));
#30902=CARTESIAN_POINT('Origin',(0.,0.,-3.6));
#30903=CARTESIAN_POINT('Origin',(0.298,0.,-3.6));
#30904=CARTESIAN_POINT('Origin',(0.,0.,0.01));
#30905=CARTESIAN_POINT('',(-0.5,-6.12323399573677E-17,0.02));
#30906=CARTESIAN_POINT('Origin',(0.,0.,0.02));
#30907=CARTESIAN_POINT('',(-0.49,-6.00076931582203E-17,0.01));
#30908=CARTESIAN_POINT('Origin',(0.,0.,0.29));
#30909=CARTESIAN_POINT('Origin',(0.,0.,0.56));
#30910=CARTESIAN_POINT('Origin',(0.,0.,0.56));
#30911=CARTESIAN_POINT('Origin',(0.,0.,0.56));
#30912=CARTESIAN_POINT('Origin',(0.,0.,0.56));
#30913=CARTESIAN_POINT('Origin',(0.,0.,0.56));
#30914=CARTESIAN_POINT('Origin',(0.,0.,0.56));
#30915=CARTESIAN_POINT('Origin',(0.,0.,0.56));
#30916=CARTESIAN_POINT('Origin',(0.,0.,0.56));
#30917=CARTESIAN_POINT('Origin',(0.,0.,0.56));
#30918=CARTESIAN_POINT('Origin',(0.,0.,0.56));
#30919=CARTESIAN_POINT('Origin',(0.,0.,0.56));
#30920=CARTESIAN_POINT('Origin',(0.,0.,0.56));
#30921=CARTESIAN_POINT('Origin',(0.,0.,0.56));
#30922=CARTESIAN_POINT('Origin',(0.,0.,0.56));
#30923=CARTESIAN_POINT('Origin',(0.,0.,0.56));
#30924=CARTESIAN_POINT('Origin',(0.,0.,0.56));
#30925=CARTESIAN_POINT('',(-0.5,-6.12323399573677E-17,0.29));
#30926=CARTESIAN_POINT('Origin',(0.,0.,0.56));
#30927=CARTESIAN_POINT('Origin',(0.,0.,0.56));
#30928=CARTESIAN_POINT('Origin',(0.,0.,0.56));
#30929=CARTESIAN_POINT('Origin',(0.,0.,0.56));
#30930=CARTESIAN_POINT('Origin',(0.,0.,0.56));
#30931=CARTESIAN_POINT('Origin',(0.,0.,0.56));
#30932=CARTESIAN_POINT('Origin',(0.,0.,0.56));
#30933=CARTESIAN_POINT('Origin',(0.,0.,0.56));
#30934=CARTESIAN_POINT('Origin',(0.,0.,0.56));
#30935=CARTESIAN_POINT('Origin',(0.,0.,0.56));
#30936=CARTESIAN_POINT('Origin',(0.,0.,0.56));
#30937=CARTESIAN_POINT('Origin',(0.,0.,0.56));
#30938=CARTESIAN_POINT('Origin',(0.,0.,0.56));
#30939=CARTESIAN_POINT('Origin',(0.,0.,0.56));
#30940=CARTESIAN_POINT('Origin',(0.,0.,0.56));
#30941=CARTESIAN_POINT('Origin',(0.,0.,0.56));
#30942=CARTESIAN_POINT('Origin',(0.,0.,0.56));
#30943=CARTESIAN_POINT('Origin',(0.,0.,0.56));
#30944=CARTESIAN_POINT('Origin',(0.,0.,0.56));
#30945=CARTESIAN_POINT('Origin',(0.,0.,0.56));
#30946=CARTESIAN_POINT('Origin',(0.,0.,0.58));
#30947=CARTESIAN_POINT('',(-0.46,-5.63337527607782E-17,0.6));
#30948=CARTESIAN_POINT('Origin',(0.,0.,0.6));
#30949=CARTESIAN_POINT('',(-0.48,-5.87830463590729E-17,0.58));
#30950=CARTESIAN_POINT('Origin',(0.,0.,0.6));
#30951=CARTESIAN_POINT('',(0.,0.,0.));
#30952=CARTESIAN_POINT('Origin',(0.,0.,0.15));
#30953=CARTESIAN_POINT('',(0.58,-7.10295143505465E-17,0.16));
#30954=CARTESIAN_POINT('Origin',(0.,0.,0.16));
#30955=CARTESIAN_POINT('',(0.6,7.34788079488412E-17,0.14));
#30956=CARTESIAN_POINT('',(0.59,7.22541611496938E-17,0.15));
#30957=CARTESIAN_POINT('',(-0.6,-7.34788079488412E-17,0.14));
#30958=CARTESIAN_POINT('Origin',(0.,0.,0.14));
#30959=CARTESIAN_POINT('Origin',(0.,0.,0.14));
#30960=CARTESIAN_POINT('Origin',(0.32,0.,0.16));
#30961=CARTESIAN_POINT('',(0.34,4.163799117101E-17,0.16));
#30962=CARTESIAN_POINT('Origin',(0.,0.,0.16));
#30963=CARTESIAN_POINT('Origin',(0.,0.,0.09));
#30964=CARTESIAN_POINT('',(-0.6,-7.34788079488412E-17,0.02));
#30965=CARTESIAN_POINT('',(-0.6,-7.34788079488412E-17,0.09));
#30966=CARTESIAN_POINT('Origin',(0.,0.,0.02));
#30967=CARTESIAN_POINT('Origin',(0.,0.,0.01));
#30968=CARTESIAN_POINT('',(0.34,-4.163799117101E-17,0.));
#30969=CARTESIAN_POINT('Origin',(0.,0.,0.));
#30970=CARTESIAN_POINT('',(0.32,3.91886975727153E-17,0.02));
#30971=CARTESIAN_POINT('',(0.33,-4.04133443718627E-17,0.01));
#30972=CARTESIAN_POINT('',(-0.32,-3.91886975727153E-17,0.02));
#30973=CARTESIAN_POINT('Origin',(0.,0.,0.02));
#30974=CARTESIAN_POINT('Origin',(0.,0.,0.02));
#30975=CARTESIAN_POINT('Origin',(0.,0.,0.08));
#30976=CARTESIAN_POINT('',(0.32,-3.91886975727153E-17,0.14));
#30977=CARTESIAN_POINT('',(-0.32,-3.91886975727153E-17,0.14));
#30978=CARTESIAN_POINT('Origin',(0.,0.,0.14));
#30979=CARTESIAN_POINT('Origin',(0.,0.,0.14));
#30980=CARTESIAN_POINT('',(-0.32,-3.91886975727153E-17,0.08));
#30981=CARTESIAN_POINT('Origin',(0.58,0.,0.));
#30982=CARTESIAN_POINT('',(-0.58,-7.10295143505465E-17,-1.73472347597681E-18));
#30983=CARTESIAN_POINT('Origin',(0.,0.,0.));
#30984=CARTESIAN_POINT('Origin',(0.,0.,0.15));
#30985=CARTESIAN_POINT('',(0.33,-4.04133443718627E-17,0.15));
#30986=CARTESIAN_POINT('Origin',(0.,0.,0.01));
#30987=CARTESIAN_POINT('',(-0.59,-7.22541611496938E-17,0.01));
#30988=CARTESIAN_POINT('',(0.,0.,0.));
#30989=CARTESIAN_POINT('Origin',(0.5,-0.267675134594871,0.445023951189801));
#30990=CARTESIAN_POINT('',(0.5,-0.267675134594871,0.445023951189801));
#30991=CARTESIAN_POINT('',(0.481813466520527,-0.299175134594813,0.445023951189787));
#30992=CARTESIAN_POINT('',(0.5,-0.267675134594813,0.445023951189788));
#30993=CARTESIAN_POINT('',(0.481096510297973,-0.277761199726725,0.473510370999757));
#30994=CARTESIAN_POINT('Ctrl Pts',(0.5,-0.267675134594871,0.445023951189802));
#30995=CARTESIAN_POINT('Ctrl Pts',(0.496851093414489,-0.269349908597711,
0.449775881890813));
#30996=CARTESIAN_POINT('Ctrl Pts',(0.493701109562143,-0.271027926795793,
0.454526079554539));
#30997=CARTESIAN_POINT('Ctrl Pts',(0.487399980032294,-0.274389929231452,
0.464021503658784));
#30998=CARTESIAN_POINT('Ctrl Pts',(0.484248729970766,-0.276073967840828,
0.468766889063092));
#30999=CARTESIAN_POINT('Ctrl Pts',(0.481096510297973,-0.277761199726724,
0.473510370999757));
#31000=CARTESIAN_POINT('Ctrl Pts',(0.481096510297973,-0.277761199726725,
0.473510370999757));
#31001=CARTESIAN_POINT('Ctrl Pts',(0.481211435993815,-0.281334765706086,
0.468766825717716));
#31002=CARTESIAN_POINT('Ctrl Pts',(0.481328642403551,-0.284905895274937,
0.46402137691612));
#31003=CARTESIAN_POINT('Ctrl Pts',(0.481567627773124,-0.292043834604859,
0.454525952714809));
#31004=CARTESIAN_POINT('Ctrl Pts',(0.481689411716076,-0.295610762084322,
0.449775818448415));
#31005=CARTESIAN_POINT('Ctrl Pts',(0.4818134665205,-0.299175134594829,0.445023951189826));
#31006=CARTESIAN_POINT('Origin',(3.40159364172662E-17,-0.555522399453449,
0.473510370999757));
#31007=CARTESIAN_POINT('',(3.40159364172662E-17,-0.555522399453449,0.473510370999757));
#31008=CARTESIAN_POINT('',(0.0181865334794225,-0.566850269189655,0.445023951189802));
#31009=CARTESIAN_POINT('Ctrl Pts',(0.0181865334794225,-0.566850269189655,
0.445023951189802));
#31010=CARTESIAN_POINT('Ctrl Pts',(0.0151616833547915,-0.564960623093991,
0.449775881890529));
#31011=CARTESIAN_POINT('Ctrl Pts',(0.0121334850409848,-0.563071666155339,
0.454526079554383));
#31012=CARTESIAN_POINT('Ctrl Pts',(0.00607134075855177,-0.559295729127382,
0.464021503659636));
#31013=CARTESIAN_POINT('Ctrl Pts',(0.00303729551137823,-0.557408685825276,
0.468766889063527));
#31014=CARTESIAN_POINT('Ctrl Pts',(-3.36036318723674E-16,-0.555522399453449,
0.473510370999756));
#31015=CARTESIAN_POINT('',(-0.0181865334794733,-0.566850269189626,0.445023951189787));
#31016=CARTESIAN_POINT('Ctrl Pts',(-2.12685567010027E-16,-0.555522399453449,
0.473510370999756));
#31017=CARTESIAN_POINT('Ctrl Pts',(-0.00303733607236141,-0.557408711015311,
0.468766825717629));
#31018=CARTESIAN_POINT('Ctrl Pts',(-0.00607142179437835,-0.559295779528088,
0.464021376915948));
#31019=CARTESIAN_POINT('Ctrl Pts',(-0.0121335658997963,-0.56307171659412,
0.454525952714919));
#31020=CARTESIAN_POINT('Ctrl Pts',(-0.015161723738915,-0.564960648322172,
0.449775818448647));
#31021=CARTESIAN_POINT('Ctrl Pts',(-0.0181865334794998,-0.56685026918961,
0.445023951189826));
#31022=CARTESIAN_POINT('',(0.018186533479473,-0.566850269189626,0.445023951189787));
#31023=CARTESIAN_POINT('Origin',(0.481813466520577,0.299175134594784,0.445023951189801));
#31024=CARTESIAN_POINT('',(0.481813466520577,0.299175134594784,0.445023951189801));
#31025=CARTESIAN_POINT('',(0.5,0.267675134594813,0.445023951189787));
#31026=CARTESIAN_POINT('',(0.481813466520527,0.299175134594813,0.445023951189788));
#31027=CARTESIAN_POINT('',(0.481096510297973,0.277761199726725,0.473510370999757));
#31028=CARTESIAN_POINT('Ctrl Pts',(0.481813466520577,0.299175134594784,
0.445023951189802));
#31029=CARTESIAN_POINT('Ctrl Pts',(0.481689410059888,0.295610714496447,
0.449775881890441));
#31030=CARTESIAN_POINT('Ctrl Pts',(0.481567624521262,0.292043739359626,
0.45452607955435));
#31031=CARTESIAN_POINT('Ctrl Pts',(0.48132863927319,0.284905799896003,0.464021503659138));
#31032=CARTESIAN_POINT('Ctrl Pts',(0.481211434459105,0.281334717984484,
0.468766889063272));
#31033=CARTESIAN_POINT('Ctrl Pts',(0.481096510297974,0.277761199726724,
0.473510370999757));
#31034=CARTESIAN_POINT('Ctrl Pts',(0.481096510297974,0.277761199726724,
0.473510370999757));
#31035=CARTESIAN_POINT('Ctrl Pts',(0.484248772066078,0.276073945309214,
0.46876682571778));
#31036=CARTESIAN_POINT('Ctrl Pts',(0.487400064197721,0.274389884253135,
0.464021376916268));
#31037=CARTESIAN_POINT('Ctrl Pts',(0.493701193672944,0.271027881989329,
0.454525952714879));
#31038=CARTESIAN_POINT('Ctrl Pts',(0.496851135455045,0.269349886237992,
0.449775818448557));
#31039=CARTESIAN_POINT('Ctrl Pts',(0.5,0.267675134594782,0.445023951189826));
#31040=CARTESIAN_POINT('Origin',(-0.481096510297974,-0.277761199726724,
0.473510370999757));
#31041=CARTESIAN_POINT('',(-0.481096510297974,-0.277761199726724,0.473510370999757));
#31042=CARTESIAN_POINT('',(-0.481813466520577,-0.299175134594784,0.445023951189802));
#31043=CARTESIAN_POINT('Ctrl Pts',(-0.481813466520578,-0.299175134594784,
0.445023951189801));
#31044=CARTESIAN_POINT('Ctrl Pts',(-0.481689410059868,-0.295610714495857,
0.449775881891228));
#31045=CARTESIAN_POINT('Ctrl Pts',(-0.481567624521253,-0.292043739359335,
0.454526079554737));
#31046=CARTESIAN_POINT('Ctrl Pts',(-0.481328639273198,-0.284905799896236,
0.464021503658828));
#31047=CARTESIAN_POINT('Ctrl Pts',(-0.481211434459109,-0.281334717984605,
0.468766889063111));
#31048=CARTESIAN_POINT('Ctrl Pts',(-0.481096510297974,-0.277761199726725,
0.473510370999757));
#31049=CARTESIAN_POINT('',(-0.5,-0.267675134594813,0.445023951189787));
#31050=CARTESIAN_POINT('Ctrl Pts',(-0.481096510297974,-0.277761199726724,
0.473510370999757));
#31051=CARTESIAN_POINT('Ctrl Pts',(-0.484248772066081,-0.276073945309212,
0.468766825717777));
#31052=CARTESIAN_POINT('Ctrl Pts',(-0.487400064197745,-0.274389884253123,
0.464021376916233));
#31053=CARTESIAN_POINT('Ctrl Pts',(-0.493701193672965,-0.271027881989318,
0.454525952714847));
#31054=CARTESIAN_POINT('Ctrl Pts',(-0.496851135455069,-0.269349886237979,
0.44977581844852));
#31055=CARTESIAN_POINT('Ctrl Pts',(-0.5,-0.267675134594782,0.445023951189826));
#31056=CARTESIAN_POINT('',(-0.481813466520527,-0.299175134594813,0.445023951189787));
#31057=CARTESIAN_POINT('Origin',(-0.0181865334794227,0.566850269189655,
0.445023951189802));
#31058=CARTESIAN_POINT('',(-0.0181865334794227,0.566850269189655,0.445023951189802));
#31059=CARTESIAN_POINT('',(0.0181865334794732,0.566850269189626,0.445023951189787));
#31060=CARTESIAN_POINT('',(-0.0181865334794732,0.566850269189626,0.445023951189788));
#31061=CARTESIAN_POINT('',(3.40159364172662E-17,0.555522399453449,0.473510370999757));
#31062=CARTESIAN_POINT('Ctrl Pts',(-0.0181865334794227,0.566850269189655,
0.445023951189802));
#31063=CARTESIAN_POINT('Ctrl Pts',(-0.0151616833546625,0.564960623093911,
0.449775881890732));
#31064=CARTESIAN_POINT('Ctrl Pts',(-0.0121334850409241,0.563071666155301,
0.454526079554478));
#31065=CARTESIAN_POINT('Ctrl Pts',(-0.00607134075884239,0.559295729127563,
0.464021503659181));
#31066=CARTESIAN_POINT('Ctrl Pts',(-0.00303729551152701,0.557408685825368,
0.468766889063295));
#31067=CARTESIAN_POINT('Ctrl Pts',(-2.12685567010027E-16,0.555522399453449,
0.473510370999757));
#31068=CARTESIAN_POINT('Ctrl Pts',(1.57366688130913E-16,0.555522399453449,
0.473510370999757));
#31069=CARTESIAN_POINT('Ctrl Pts',(0.00303733607213158,0.557408711015168,
0.468766825717988));
#31070=CARTESIAN_POINT('Ctrl Pts',(0.00607142179389414,0.559295779527786,
0.464021376916707));
#31071=CARTESIAN_POINT('Ctrl Pts',(0.012133565899859,0.563071716594158,
0.454525952714821));
#31072=CARTESIAN_POINT('Ctrl Pts',(0.015161723739062,0.564960648322264,
0.449775818448416));
#31073=CARTESIAN_POINT('Ctrl Pts',(0.0181865334794999,0.56685026918961,
0.445023951189826));
#31074=CARTESIAN_POINT('Origin',(-0.481096510297974,0.277761199726725,0.473510370999757));
#31075=CARTESIAN_POINT('',(-0.481096510297974,0.277761199726725,0.473510370999757));
#31076=CARTESIAN_POINT('',(-0.5,0.267675134594871,0.445023951189801));
#31077=CARTESIAN_POINT('Ctrl Pts',(-0.5,0.267675134594871,0.445023951189802));
#31078=CARTESIAN_POINT('Ctrl Pts',(-0.496851093414684,0.269349908597607,
0.44977588189052));
#31079=CARTESIAN_POINT('Ctrl Pts',(-0.493701109562242,0.271027926795741,
0.45452607955439));
#31080=CARTESIAN_POINT('Ctrl Pts',(-0.487399980032028,0.274389929231594,
0.464021503659185));
#31081=CARTESIAN_POINT('Ctrl Pts',(-0.484248729970629,0.276073967840903,
0.468766889063299));
#31082=CARTESIAN_POINT('Ctrl Pts',(-0.481096510297974,0.277761199726725,
0.473510370999757));
#31083=CARTESIAN_POINT('',(-0.481813466520527,0.299175134594813,0.445023951189787));
#31084=CARTESIAN_POINT('Ctrl Pts',(-0.481096510297974,0.277761199726724,
0.473510370999757));
#31085=CARTESIAN_POINT('Ctrl Pts',(-0.481211435993815,0.281334765706079,
0.468766825717724));
#31086=CARTESIAN_POINT('Ctrl Pts',(-0.48132864240355,0.284905895274894,
0.464021376916177));
#31087=CARTESIAN_POINT('Ctrl Pts',(-0.48156762777312,0.292043834604734,
0.454525952714975));
#31088=CARTESIAN_POINT('Ctrl Pts',(-0.481689411716068,0.295610762084098,
0.449775818448714));
#31089=CARTESIAN_POINT('Ctrl Pts',(-0.4818134665205,0.299175134594828,0.445023951189826));
#31090=CARTESIAN_POINT('',(-0.5,0.267675134594813,0.445023951189788));
#31091=CARTESIAN_POINT('Ctrl Pts',(-0.483544441026001,0.298175755998117,
0.444468924013264));
#31092=CARTESIAN_POINT('Ctrl Pts',(-0.406912985802199,0.342418947299972,
0.469110141953084));
#31093=CARTESIAN_POINT('Ctrl Pts',(-0.257908341391985,0.428446818860713,
0.495972649874704));
#31094=CARTESIAN_POINT('Ctrl Pts',(-0.118630832605733,0.508858726050516,
0.477323881266358));
#31095=CARTESIAN_POINT('Ctrl Pts',(-0.0164555589739993,0.567849647786322,
0.444468924013264));
#31096=CARTESIAN_POINT('Ctrl Pts',(-0.482728464116659,0.291370903907653,
0.454149406342095));
#31097=CARTESIAN_POINT('Ctrl Pts',(-0.405668349322323,0.335995410650277,
0.479195744603699));
#31098=CARTESIAN_POINT('Ctrl Pts',(-0.255104666887408,0.42318499384238,
0.506818674741199));
#31099=CARTESIAN_POINT('Ctrl Pts',(-0.113871724472838,0.504508880129862,
0.487544524024234));
#31100=CARTESIAN_POINT('Ctrl Pts',(-0.0109703726493329,0.563740565008697,
0.454149406342095));
#31101=CARTESIAN_POINT('Ctrl Pts',(-0.481912487207316,0.284566051817189,
0.463829888670926));
#31102=CARTESIAN_POINT('Ctrl Pts',(-0.404423712842447,0.329571874000582,
0.489281347254314));
#31103=CARTESIAN_POINT('Ctrl Pts',(-0.252300992382831,0.417923168824047,
0.517664699607693));
#31104=CARTESIAN_POINT('Ctrl Pts',(-0.109112616339942,0.500159034209207,
0.49776516678211));
#31105=CARTESIAN_POINT('Ctrl Pts',(-0.00548518632466643,0.559631482231073,
0.463829888670926));
#31106=CARTESIAN_POINT('Ctrl Pts',(-0.481096510297974,0.277761199726724,
0.473510370999756));
#31107=CARTESIAN_POINT('Ctrl Pts',(-0.403179076362571,0.323148337350887,
0.499366949904929));
#31108=CARTESIAN_POINT('Ctrl Pts',(-0.249497317878254,0.412661343805713,
0.528510724474188));
#31109=CARTESIAN_POINT('Ctrl Pts',(-0.104353508207047,0.495809188288553,
0.507985809539986));
#31110=CARTESIAN_POINT('Ctrl Pts',(1.38777878078145E-17,0.555522399453449,
0.473510370999757));
#31111=CARTESIAN_POINT('',(-0.332273583321365,0.364361108482639,0.50952199081629));
#31112=CARTESIAN_POINT('',(-0.149406387802791,0.469927086065252,0.50977488582138));
#31113=CARTESIAN_POINT('Ctrl Pts',(-0.332255993860912,0.364371421655621,
0.509523338656206));
#31114=CARTESIAN_POINT('Ctrl Pts',(-0.318279946918584,0.373351253352375,
0.510249567790552));
#31115=CARTESIAN_POINT('Ctrl Pts',(-0.304245988201247,0.38215746972964,
0.510799578547925));
#31116=CARTESIAN_POINT('Ctrl Pts',(-0.290111717192355,0.390806403397501,
0.511195921402465));
#31117=CARTESIAN_POINT('Ctrl Pts',(-0.287860051912662,0.392184224979812,
0.511259060947749));
#31118=CARTESIAN_POINT('Ctrl Pts',(-0.28560575614068,0.393558099738657,
0.511318349002632));
#31119=CARTESIAN_POINT('Ctrl Pts',(-0.283348567387494,0.394928140744563,
0.511373928077867));
#31120=CARTESIAN_POINT('Ctrl Pts',(-0.280216737305738,0.39682906091771,
0.511451043569202));
#31121=CARTESIAN_POINT('Ctrl Pts',(-0.277081273935527,0.398721437766428,
0.511520951504384));
#31122=CARTESIAN_POINT('Ctrl Pts',(-0.273941641913879,0.400605537752242,
0.511584044834106));
#31123=CARTESIAN_POINT('Ctrl Pts',(-0.267927330155416,0.404214739283079,
0.511704907072805));
#31124=CARTESIAN_POINT('Ctrl Pts',(-0.261897755700511,0.407793556450529,
0.511800747922412));
#31125=CARTESIAN_POINT('Ctrl Pts',(-0.25584883066306,0.411344203910499,
0.511868640474087));
#31126=CARTESIAN_POINT('Ctrl Pts',(-0.248348767769815,0.415746652130082,
0.511952820457207));
#31127=CARTESIAN_POINT('Ctrl Pts',(-0.240826093245991,0.420101623101484,
0.511993883112242));
#31128=CARTESIAN_POINT('Ctrl Pts',(-0.233273179007016,0.424413640109889,
0.511986957182662));
#31129=CARTESIAN_POINT('Ctrl Pts',(-0.224651569134181,0.429335783700459,
0.511979051272312));
#31130=CARTESIAN_POINT('Ctrl Pts',(-0.215999456170061,0.434196874243185,
0.511908560978455));
#31131=CARTESIAN_POINT('Ctrl Pts',(-0.207306027932602,0.439003856133907,
0.511770158465883));
#31132=CARTESIAN_POINT('Ctrl Pts',(-0.192599818167039,0.44713557150479,
0.511536030303048));
#31133=CARTESIAN_POINT('Ctrl Pts',(-0.17781016961573,0.455093185534583,
0.511107142930621));
#31134=CARTESIAN_POINT('Ctrl Pts',(-0.162894469075894,0.462908436068343,
0.51047380092448));
#31135=CARTESIAN_POINT('Ctrl Pts',(-0.15843407026544,0.465245512633475,
0.510284406003118));
#31136=CARTESIAN_POINT('Ctrl Pts',(-0.153964937425956,0.467568528701837,
0.51007694825866));
#31137=CARTESIAN_POINT('Ctrl Pts',(-0.149486235114875,0.469878234401755,
0.509851518489547));
#31138=CARTESIAN_POINT('Ctrl Pts',(-0.149486235113333,0.46987823440264,
0.50985151848933));
#31139=CARTESIAN_POINT('Ctrl Pts',(-0.10320209198028,0.496453452351216,
0.503326883310332));
#31140=CARTESIAN_POINT('Ctrl Pts',(-0.0545240825613662,0.524322604530414,
0.491523580997232));
#31141=CARTESIAN_POINT('Ctrl Pts',(1.38777878078145E-17,0.555522399453449,
0.473510370999757));
#31142=CARTESIAN_POINT('Ctrl Pts',(-0.0181867260015379,0.56685015803696,
0.44502415632149));
#31143=CARTESIAN_POINT('Ctrl Pts',(-0.119531026231089,0.508338999018595,
0.47744392523402));
#31144=CARTESIAN_POINT('Ctrl Pts',(-0.257939671025404,0.428428730688425,
0.495826064932766));
#31145=CARTESIAN_POINT('Ctrl Pts',(-0.405950132909958,0.342974850676497,
0.469283267869301));
#31146=CARTESIAN_POINT('Ctrl Pts',(-0.48181328528966,0.299175239228503,
0.445024047543947));
#31147=CARTESIAN_POINT('Ctrl Pts',(-0.481096510297974,0.277761199726724,
0.473510370999756));
#31148=CARTESIAN_POINT('Ctrl Pts',(-0.426814654021077,0.309380542881391,
0.491523580997232));
#31149=CARTESIAN_POINT('Ctrl Pts',(-0.378382919626527,0.337590700753812,
0.503049636797564));
#31150=CARTESIAN_POINT('Ctrl Pts',(-0.332255993862453,0.364371421654726,
0.50952333865599));
#31151=CARTESIAN_POINT('Origin',(-0.490906733260264,0.283425134594813,0.));
#31152=CARTESIAN_POINT('',(-0.481813466520527,0.299175134594813,0.0531981726275096));
#31153=CARTESIAN_POINT('',(-0.5,0.267675134594813,0.0531981726275097));
#31154=CARTESIAN_POINT('Ctrl Pts',(-0.481813466520527,0.299175134594813,
0.0531981726275096));
#31155=CARTESIAN_POINT('Ctrl Pts',(-0.490906733260264,0.283425134594813,
0.0528614692578827));
#31156=CARTESIAN_POINT('Ctrl Pts',(-0.5,0.267675134594813,0.0531981726275097));
#31157=CARTESIAN_POINT('',(-0.5,0.267675134594813,0.));
#31158=CARTESIAN_POINT('',(-0.481813466520527,0.299175134594813,0.));
#31159=CARTESIAN_POINT('Ctrl Pts',(-0.5,-0.269673891788205,0.444468924013264));
#31160=CARTESIAN_POINT('Ctrl Pts',(-0.5,-0.181187509184495,0.469110141953084));
#31161=CARTESIAN_POINT('Ctrl Pts',(-0.5,-0.00912777933363359,0.495992583115463));
#31162=CARTESIAN_POINT('Ctrl Pts',(-0.5,0.151692048316594,0.477323881266358));
#31163=CARTESIAN_POINT('Ctrl Pts',(-0.5,0.269673891788205,0.444468924013264));
#31164=CARTESIAN_POINT('Ctrl Pts',(-0.493698836765991,-0.272369661101045,
0.454149406342095));
#31165=CARTESIAN_POINT('Ctrl Pts',(-0.493814735839286,-0.183321390699293,
0.479195744603699));
#31166=CARTESIAN_POINT('Ctrl Pts',(-0.494041168132572,-0.00933048749449408,
0.506838267803536));
#31167=CARTESIAN_POINT('Ctrl Pts',(-0.493853368863718,0.153638633898712,
0.487544524024234));
#31168=CARTESIAN_POINT('Ctrl Pts',(-0.493698836765991,0.272369661101045,
0.454149406342095));
#31169=CARTESIAN_POINT('Ctrl Pts',(-0.487397673531982,-0.275065430413885,
0.463829888670926));
#31170=CARTESIAN_POINT('Ctrl Pts',(-0.487629471678572,-0.185455272214091,
0.489281347254314));
#31171=CARTESIAN_POINT('Ctrl Pts',(-0.488082336265144,-0.00953319565535434,
0.517683952491609));
#31172=CARTESIAN_POINT('Ctrl Pts',(-0.487706737727435,0.155585219480829,
0.49776516678211));
#31173=CARTESIAN_POINT('Ctrl Pts',(-0.487397673531982,0.275065430413885,
0.463829888670926));
#31174=CARTESIAN_POINT('Ctrl Pts',(-0.481096510297973,-0.277761199726725,
0.473510370999757));
#31175=CARTESIAN_POINT('Ctrl Pts',(-0.481444207517858,-0.187589153728889,
0.499366949904929));
#31176=CARTESIAN_POINT('Ctrl Pts',(-0.482123504397716,-0.00973590381621485,
0.528529637179682));
#31177=CARTESIAN_POINT('Ctrl Pts',(-0.481560106591152,0.157531805062946,
0.507985809539986));
#31178=CARTESIAN_POINT('Ctrl Pts',(-0.481096510297974,0.277761199726725,
0.473510370999757));
#31179=CARTESIAN_POINT('',(-0.48168265812218,-0.105573547381759,0.509528465790875));
#31180=CARTESIAN_POINT('',(-0.481671866090386,0.105573308103865,0.509780497494418));
#31181=CARTESIAN_POINT('Ctrl Pts',(-0.481682776226655,-0.105554844793129,
0.509530050599285));
#31182=CARTESIAN_POINT('Ctrl Pts',(-0.482471555403153,-0.0889600413291659,
0.510257198470763));
#31183=CARTESIAN_POINT('Ctrl Pts',(-0.483081002674462,-0.0724019202065436,
0.510808016142969));
#31184=CARTESIAN_POINT('Ctrl Pts',(-0.48350406187927,-0.0558356242392143,
0.511204872441748));
#31185=CARTESIAN_POINT('Ctrl Pts',(-0.483571425521599,-0.0531977758634472,
0.511268063799986));
#31186=CARTESIAN_POINT('Ctrl Pts',(-0.483634059821167,-0.0505596245392988,
0.511327399849453));
#31187=CARTESIAN_POINT('Ctrl Pts',(-0.483691931501727,-0.047920886921818,
0.511383022134839));
#31188=CARTESIAN_POINT('Ctrl Pts',(-0.48377226082532,-0.0442581626687918,
0.511460229164573));
#31189=CARTESIAN_POINT('Ctrl Pts',(-0.483843374961778,-0.0405965669336863,
0.511530213514606));
#31190=CARTESIAN_POINT('Ctrl Pts',(-0.483905237009646,-0.0369355032943481,
0.511593366062782));
#31191=CARTESIAN_POINT('Ctrl Pts',(-0.484023740592018,-0.0299223317052114,
0.511714341740967));
#31192=CARTESIAN_POINT('Ctrl Pts',(-0.484108299964325,-0.0229111484510916,
0.511810232838511));
#31193=CARTESIAN_POINT('Ctrl Pts',(-0.484158788944568,-0.0158973041957685,
0.511878119719765));
#31194=CARTESIAN_POINT('Ctrl Pts',(-0.484221390237341,-0.00720083784635109,
0.511962292672129));
#31195=CARTESIAN_POINT('Ctrl Pts',(-0.484231570102655,0.00149145331024759,
0.512003262320269));
#31196=CARTESIAN_POINT('Ctrl Pts',(-0.484189431542939,0.010188440724828,
0.511996173735513));
#31197=CARTESIAN_POINT('Ctrl Pts',(-0.484141330609844,0.0201160038064456,
0.51198808215518));
#31198=CARTESIAN_POINT('Ctrl Pts',(-0.484025105493291,0.0300394371693865,
0.511917315710112));
#31199=CARTESIAN_POINT('Ctrl Pts',(-0.483841363935383,0.0399715823347925,
0.511778573331064));
#31200=CARTESIAN_POINT('Ctrl Pts',(-0.483530538123121,0.0567732635858149,
0.511543870234205));
#31201=CARTESIAN_POINT('Ctrl Pts',(-0.483027218617348,0.0735601148901351,
0.511114228132524));
#31202=CARTESIAN_POINT('Ctrl Pts',(-0.482337584156177,0.0903849359947383,
0.510480081135851));
#31203=CARTESIAN_POINT('Ctrl Pts',(-0.482131355509923,0.0954162392071141,
0.510290445489704));
#31204=CARTESIAN_POINT('Ctrl Pts',(-0.481908583230074,0.100448074937233,
0.510082742562517));
#31205=CARTESIAN_POINT('Ctrl Pts',(-0.481669499211642,0.105481542418297,
0.509857066299145));
#31206=CARTESIAN_POINT('Ctrl Pts',(-0.481669499211638,0.105481542420091,
0.509857066298925));
#31207=CARTESIAN_POINT('Ctrl Pts',(-0.481542291138614,0.158851785396327,
0.503329833692243));
#31208=CARTESIAN_POINT('Ctrl Pts',(-0.481338736582444,0.214942061649024,
0.491523580997232));
#31209=CARTESIAN_POINT('Ctrl Pts',(-0.481096510297974,0.277761199726725,
0.473510370999757));
#31210=CARTESIAN_POINT('Ctrl Pts',(-0.5,0.267674912507137,0.445024157409747));
#31211=CARTESIAN_POINT('Ctrl Pts',(-0.5,0.150652619934056,0.47744405363793));
#31212=CARTESIAN_POINT('Ctrl Pts',(-0.5,-0.00916398135951556,0.495845869769615));
#31213=CARTESIAN_POINT('Ctrl Pts',(-0.5,-0.180075676750139,0.469283396273211));
#31214=CARTESIAN_POINT('Ctrl Pts',(-0.5,-0.267674925037408,0.44502404899404));
#31215=CARTESIAN_POINT('Ctrl Pts',(-0.481096510297973,-0.277761199726725,
0.473510370999757));
#31216=CARTESIAN_POINT('Ctrl Pts',(-0.481338736582444,-0.214942061649024,
0.491523580997232));
#31217=CARTESIAN_POINT('Ctrl Pts',(-0.481553507568566,-0.158892946912006,
0.503053570640112));
#31218=CARTESIAN_POINT('Ctrl Pts',(-0.481682776226651,-0.105554844794932,
0.509530050599066));
#31219=CARTESIAN_POINT('Ctrl Pts',(0.0164555589739993,0.567849647786322,
0.444468924013264));
#31220=CARTESIAN_POINT('Ctrl Pts',(0.093087014197801,0.523606456484467,
0.469110141953085));
#31221=CARTESIAN_POINT('Ctrl Pts',(0.242091658608015,0.437578584923725,
0.495972649874704));
#31222=CARTESIAN_POINT('Ctrl Pts',(0.381369167394267,0.357166677733922,
0.477323881266358));
#31223=CARTESIAN_POINT('Ctrl Pts',(0.483544441026001,0.298175755998117,
0.444468924013264));
#31224=CARTESIAN_POINT('Ctrl Pts',(0.0109703726493329,0.563740565008697,
0.454149406342095));
#31225=CARTESIAN_POINT('Ctrl Pts',(0.0881463865169628,0.51931680134957,
0.479195744603699));
#31226=CARTESIAN_POINT('Ctrl Pts',(0.238936621724158,0.432519619069652,
0.506818674741199));
#31227=CARTESIAN_POINT('Ctrl Pts',(0.37998164439088,0.350870246231151,0.487544524024234));
#31228=CARTESIAN_POINT('Ctrl Pts',(0.482728464116658,0.291370903907653,
0.454149406342095));
#31229=CARTESIAN_POINT('Ctrl Pts',(0.00548518632466648,0.559631482231073,
0.463829888670926));
#31230=CARTESIAN_POINT('Ctrl Pts',(0.0832057588361247,0.515027146214673,
0.489281347254314));
#31231=CARTESIAN_POINT('Ctrl Pts',(0.235781584840302,0.427460653215579,
0.517664699607693));
#31232=CARTESIAN_POINT('Ctrl Pts',(0.378594121387492,0.344573814728379,
0.49776516678211));
#31233=CARTESIAN_POINT('Ctrl Pts',(0.481912487207316,0.284566051817189,
0.463829888670926));
#31234=CARTESIAN_POINT('Ctrl Pts',(6.93889390390723E-17,0.555522399453449,
0.473510370999757));
#31235=CARTESIAN_POINT('Ctrl Pts',(0.0782651311552866,0.510737491079776,
0.499366949904929));
#31236=CARTESIAN_POINT('Ctrl Pts',(0.232626547956445,0.422401687361506,
0.528510724474188));
#31237=CARTESIAN_POINT('Ctrl Pts',(0.377206598384105,0.338277383225607,
0.507985809539986));
#31238=CARTESIAN_POINT('Ctrl Pts',(0.481096510297974,0.277761199726724,
0.473510370999756));
#31239=CARTESIAN_POINT('',(0.149409184436338,0.469937918404108,0.509521990816289));
#31240=CARTESIAN_POINT('',(0.332265600557506,0.364353270357514,0.509774885821379));
#31241=CARTESIAN_POINT('Ctrl Pts',(0.149426910636359,0.469927842071009,
0.509523338656205));
#31242=CARTESIAN_POINT('Ctrl Pts',(0.16419169647835,0.462314146222986,0.510249567790538));
#31243=CARTESIAN_POINT('Ctrl Pts',(0.178835082930703,0.454563489646878,
0.510799578547905));
#31244=CARTESIAN_POINT('Ctrl Pts',(0.193392414706915,0.446647318723277,
0.511195921402444));
#31245=CARTESIAN_POINT('Ctrl Pts',(0.195711475839183,0.44538623018126,0.511259060947736));
#31246=CARTESIAN_POINT('Ctrl Pts',(0.198028434168209,0.444120890154363,
0.511318349002625));
#31247=CARTESIAN_POINT('Ctrl Pts',(0.200343518860398,0.442851127855779,
0.511373928077867));
#31248=CARTESIAN_POINT('Ctrl Pts',(0.20355567906179,0.441089343531216,0.511451043569201));
#31249=CARTESIAN_POINT('Ctrl Pts',(0.206762257171419,0.439320141024336,
0.511520951504384));
#31250=CARTESIAN_POINT('Ctrl Pts',(0.209963751633228,0.43754318992796,0.511584044834106));
#31251=CARTESIAN_POINT('Ctrl Pts',(0.216096567725542,0.43413924392427,0.511704907072804));
#31252=CARTESIAN_POINT('Ctrl Pts',(0.222210701535505,0.430706887856039,
0.511800747922412));
#31253=CARTESIAN_POINT('Ctrl Pts',(0.228310114954446,0.427243688838005,
0.511868640474087));
#31254=CARTESIAN_POINT('Ctrl Pts',(0.235872778398072,0.422949667952265,
0.511952820457207));
#31255=CARTESIAN_POINT('Ctrl Pts',(0.243405631153963,0.418612326195932,
0.511993883112242));
#31256=CARTESIAN_POINT('Ctrl Pts',(0.250916404544279,0.414227319096577,
0.511986957182662));
#31257=CARTESIAN_POINT('Ctrl Pts',(0.259489910871209,0.409221857720465,
0.511979051272313));
#31258=CARTESIAN_POINT('Ctrl Pts',(0.26802579525337,0.404159453368485,0.511908560978455));
#31259=CARTESIAN_POINT('Ctrl Pts',(0.276535477804989,0.399034214614234,
0.511770158465883));
#31260=CARTESIAN_POINT('Ctrl Pts',(0.290930854775299,0.390364121049316,
0.511536030303048));
#31261=CARTESIAN_POINT('Ctrl Pts',(0.305217174954266,0.381534716705735,
0.511107142930622));
#31262=CARTESIAN_POINT('Ctrl Pts',(0.319443230723362,0.372524966389875,
0.510473800924481));
#31263=CARTESIAN_POINT('Ctrl Pts',(0.323697397804576,0.369830685991582,
0.510284406003119));
#31264=CARTESIAN_POINT('Ctrl Pts',(0.327943755152913,0.367121811453886,
0.510076948258661));
#31265=CARTESIAN_POINT('Ctrl Pts',(0.332183370119856,0.364397994326456,
0.509851518489548));
#31266=CARTESIAN_POINT('Ctrl Pts',(0.332183370121399,0.36439799432556,0.50985151848933));
#31267=CARTESIAN_POINT('Ctrl Pts',(0.3783402555425,0.337602359554229,0.503326883310332));
#31268=CARTESIAN_POINT('Ctrl Pts',(0.426814654021077,0.30938054288139,0.491523580997232));
#31269=CARTESIAN_POINT('Ctrl Pts',(0.481096510297974,0.277761199726724,
0.473510370999756));
#31270=CARTESIAN_POINT('Ctrl Pts',(0.481813273998462,0.299175245747479,
0.44502415632149));
#31271=CARTESIAN_POINT('Ctrl Pts',(0.380468973768911,0.357686404765844,
0.47744392523402));
#31272=CARTESIAN_POINT('Ctrl Pts',(0.242060328974596,0.437596673096014,
0.495826064932766));
#31273=CARTESIAN_POINT('Ctrl Pts',(0.0940498670900422,0.523050553107941,
0.469283267869301));
#31274=CARTESIAN_POINT('Ctrl Pts',(0.0181867147103404,0.566850164555936,
0.445024047543947));
#31275=CARTESIAN_POINT('Ctrl Pts',(6.93889390390723E-17,0.555522399453449,
0.473510370999757));
#31276=CARTESIAN_POINT('Ctrl Pts',(0.0545240825613667,0.524322604530414,
0.491523580997232));
#31277=CARTESIAN_POINT('Ctrl Pts',(0.103170663120928,0.496484571131604,
0.503049636797564));
#31278=CARTESIAN_POINT('Ctrl Pts',(0.149426910634818,0.469927842071894,
0.50952333865599));
#31279=CARTESIAN_POINT('Origin',(-1.56125112837913E-17,0.566850269189626,
0.));
#31280=CARTESIAN_POINT('',(0.0181865334794732,0.566850269189626,0.0531981726275096));
#31281=CARTESIAN_POINT('',(-0.0181865334794732,0.566850269189626,0.0531981726275097));
#31282=CARTESIAN_POINT('Ctrl Pts',(0.0181865334794732,0.566850269189626,
0.0531981726275096));
#31283=CARTESIAN_POINT('Ctrl Pts',(-8.32667268468867E-17,0.566850269189626,
0.0528614692578828));
#31284=CARTESIAN_POINT('Ctrl Pts',(-0.0181865334794732,0.566850269189626,
0.0531981726275097));
#31285=CARTESIAN_POINT('',(-0.0181865334794732,0.566850269189626,0.));
#31286=CARTESIAN_POINT('',(0.0181865334794732,0.566850269189626,0.));
#31287=CARTESIAN_POINT('Origin',(-0.490906733260263,-0.283425134594813,
0.));
#31288=CARTESIAN_POINT('',(-0.5,-0.267675134594813,0.0531981726275096));
#31289=CARTESIAN_POINT('',(-0.481813466520527,-0.299175134594813,0.0531981726275097));
#31290=CARTESIAN_POINT('Ctrl Pts',(-0.5,-0.267675134594813,0.0531981726275096));
#31291=CARTESIAN_POINT('Ctrl Pts',(-0.490906733260263,-0.283425134594813,
0.0528614692578827));
#31292=CARTESIAN_POINT('Ctrl Pts',(-0.481813466520527,-0.299175134594813,
0.0531981726275097));
#31293=CARTESIAN_POINT('',(-0.481813466520527,-0.299175134594813,0.));
#31294=CARTESIAN_POINT('',(-0.5,-0.267675134594813,0.));
#31295=CARTESIAN_POINT('Ctrl Pts',(-0.0164555589739992,-0.567849647786322,
0.444468924013264));
#31296=CARTESIAN_POINT('Ctrl Pts',(-0.118630832605735,-0.508858726050516,
0.477323881266358));
#31297=CARTESIAN_POINT('Ctrl Pts',(-0.257908341391988,-0.428446818860712,
0.495972649874704));
#31298=CARTESIAN_POINT('Ctrl Pts',(-0.4069129858022,-0.342418947299971,
0.469110141953084));
#31299=CARTESIAN_POINT('Ctrl Pts',(-0.483544441026001,-0.298175755998117,
0.444468924013264));
#31300=CARTESIAN_POINT('Ctrl Pts',(-0.0109703726493328,-0.563740565008698,
0.454149406342095));
#31301=CARTESIAN_POINT('Ctrl Pts',(-0.113871724472839,-0.504508880129861,
0.487544524024234));
#31302=CARTESIAN_POINT('Ctrl Pts',(-0.255104666887411,-0.423184993842378,
0.506818674741198));
#31303=CARTESIAN_POINT('Ctrl Pts',(-0.405668349322324,-0.335995410650276,
0.479195744603699));
#31304=CARTESIAN_POINT('Ctrl Pts',(-0.482728464116658,-0.291370903907653,
0.454149406342095));
#31305=CARTESIAN_POINT('Ctrl Pts',(-0.00548518632466635,-0.559631482231073,
0.463829888670926));
#31306=CARTESIAN_POINT('Ctrl Pts',(-0.109112616339944,-0.500159034209207,
0.49776516678211));
#31307=CARTESIAN_POINT('Ctrl Pts',(-0.252300992382833,-0.417923168824045,
0.517664699607693));
#31308=CARTESIAN_POINT('Ctrl Pts',(-0.404423712842448,-0.329571874000581,
0.489281347254314));
#31309=CARTESIAN_POINT('Ctrl Pts',(-0.481912487207316,-0.284566051817189,
0.463829888670926));
#31310=CARTESIAN_POINT('Ctrl Pts',(5.55111512312578E-17,-0.555522399453449,
0.473510370999757));
#31311=CARTESIAN_POINT('Ctrl Pts',(-0.104353508207049,-0.495809188288552,
0.507985809539987));
#31312=CARTESIAN_POINT('Ctrl Pts',(-0.249497317878256,-0.412661343805712,
0.528510724474188));
#31313=CARTESIAN_POINT('Ctrl Pts',(-0.403179076362572,-0.323148337350886,
0.499366949904929));
#31314=CARTESIAN_POINT('Ctrl Pts',(-0.481096510297974,-0.277761199726725,
0.473510370999757));
#31315=CARTESIAN_POINT('',(-0.149406387802817,-0.469927086065238,0.509774885821372));
#31316=CARTESIAN_POINT('',(-0.332273583321351,-0.36436110848265,0.509521990816249));
#31317=CARTESIAN_POINT('Ctrl Pts',(-0.149486235114913,-0.469878234401734,
0.509851518489553));
#31318=CARTESIAN_POINT('Ctrl Pts',(-0.164305299506581,-0.462235914123333,
0.510597417196866));
#31319=CARTESIAN_POINT('Ctrl Pts',(-0.179001946260328,-0.454456869632082,
0.511144655182254));
#31320=CARTESIAN_POINT('Ctrl Pts',(-0.193610659347279,-0.446513425625821,
0.511496368941397));
#31321=CARTESIAN_POINT('Ctrl Pts',(-0.195885616680319,-0.445276424386624,
0.511551139939412));
#31322=CARTESIAN_POINT('Ctrl Pts',(-0.198158519935459,-0.444035387571388,
0.511601214129389));
#31323=CARTESIAN_POINT('Ctrl Pts',(-0.200429580583077,-0.442790159279922,
0.511646650667282));
#31324=CARTESIAN_POINT('Ctrl Pts',(-0.209799043912681,-0.437652858862111,
0.511834103158284));
#31325=CARTESIAN_POINT('Ctrl Pts',(-0.219120102170151,-0.432453709590706,
0.511941841246582));
#31326=CARTESIAN_POINT('Ctrl Pts',(-0.228405904398673,-0.427184085359904,
0.511975832565739));
#31327=CARTESIAN_POINT('Ctrl Pts',(-0.235970467119967,-0.422891251845842,
0.512003523169029));
#31328=CARTESIAN_POINT('Ctrl Pts',(-0.243504550902669,-0.418555670166371,
0.511982313941876));
#31329=CARTESIAN_POINT('Ctrl Pts',(-0.251015753293323,-0.414172765833714,
0.511916847499714));
#31330=CARTESIAN_POINT('Ctrl Pts',(-0.258685985372186,-0.409697065185204,
0.511849994980152));
#31331=CARTESIAN_POINT('Ctrl Pts',(-0.26632524258338,-0.40517616383449,
0.511737089964109));
#31332=CARTESIAN_POINT('Ctrl Pts',(-0.2739416447187,-0.400605543537466,
0.511584033754542));
#31333=CARTESIAN_POINT('Ctrl Pts',(-0.274839066022866,-0.400066998965511,
0.511565999530408));
#31334=CARTESIAN_POINT('Ctrl Pts',(-0.275736168344317,-0.399527764729909,
0.511547408980238));
#31335=CARTESIAN_POINT('Ctrl Pts',(-0.276632964213637,-0.3989878343978,
0.511528252667955));
#31336=CARTESIAN_POINT('Ctrl Pts',(-0.291025308731488,-0.390322692617817,
0.511220820112226));
#31337=CARTESIAN_POINT('Ctrl Pts',(-0.305305244489192,-0.381498545649502,
0.510766837024551));
#31338=CARTESIAN_POINT('Ctrl Pts',(-0.319523357654944,-0.372493888356987,
0.510136230701218));
#31339=CARTESIAN_POINT('Ctrl Pts',(-0.32377514957593,-0.36980113097904,
0.50994765385986));
#31340=CARTESIAN_POINT('Ctrl Pts',(-0.328018991519792,-0.367093762821116,
0.509743503525081));
#31341=CARTESIAN_POINT('Ctrl Pts',(-0.332255993860885,-0.364371421655637,
0.50952333865621));
#31342=CARTESIAN_POINT('Ctrl Pts',(-0.332255993862454,-0.364371421654726,
0.50952333865599));
#31343=CARTESIAN_POINT('Ctrl Pts',(-0.378382919626528,-0.337590700753811,
0.503049636797564));
#31344=CARTESIAN_POINT('Ctrl Pts',(-0.426814654021078,-0.30938054288139,
0.491523580997232));
#31345=CARTESIAN_POINT('Ctrl Pts',(-0.481096510297974,-0.277761199726725,
0.473510370999757));
#31346=CARTESIAN_POINT('Ctrl Pts',(-0.481813285289703,-0.299175239228478,
0.445024047543933));
#31347=CARTESIAN_POINT('Ctrl Pts',(-0.405950132909983,-0.342974850676483,
0.469283267869296));
#31348=CARTESIAN_POINT('Ctrl Pts',(-0.257939671025431,-0.42842873068841,
0.495826064932765));
#31349=CARTESIAN_POINT('Ctrl Pts',(-0.119531026231113,-0.508338999018581,
0.477443925234023));
#31350=CARTESIAN_POINT('Ctrl Pts',(-0.0181867260015819,-0.566850158036935,
0.445024156321504));
#31351=CARTESIAN_POINT('Ctrl Pts',(5.55111512312578E-17,-0.555522399453449,
0.473510370999757));
#31352=CARTESIAN_POINT('Ctrl Pts',(-0.0545240825613664,-0.524322604530414,
0.491523580997232));
#31353=CARTESIAN_POINT('Ctrl Pts',(-0.103202091980281,-0.496453452351216,
0.503326883310332));
#31354=CARTESIAN_POINT('Ctrl Pts',(-0.149486235113333,-0.46987823440264,
0.50985151848933));
#31355=CARTESIAN_POINT('Ctrl Pts',(0.5,0.269673891788205,0.444468924013264));
#31356=CARTESIAN_POINT('Ctrl Pts',(0.5,0.151692048316592,0.477323881266358));
#31357=CARTESIAN_POINT('Ctrl Pts',(0.5,-0.00912777933363709,0.495992583115463));
#31358=CARTESIAN_POINT('Ctrl Pts',(0.5,-0.181187509184497,0.469110141953084));
#31359=CARTESIAN_POINT('Ctrl Pts',(0.5,-0.269673891788205,0.444468924013264));
#31360=CARTESIAN_POINT('Ctrl Pts',(0.493698836765991,0.272369661101045,
0.454149406342095));
#31361=CARTESIAN_POINT('Ctrl Pts',(0.493853368863718,0.153638633898709,
0.487544524024234));
#31362=CARTESIAN_POINT('Ctrl Pts',(0.494041168132572,-0.00933048749449758,
0.506838267803537));
#31363=CARTESIAN_POINT('Ctrl Pts',(0.493814735839286,-0.183321390699295,
0.479195744603699));
#31364=CARTESIAN_POINT('Ctrl Pts',(0.493698836765991,-0.272369661101045,
0.454149406342095));
#31365=CARTESIAN_POINT('Ctrl Pts',(0.487397673531982,0.275065430413885,
0.463829888670926));
#31366=CARTESIAN_POINT('Ctrl Pts',(0.487706737727435,0.155585219480827,
0.49776516678211));
#31367=CARTESIAN_POINT('Ctrl Pts',(0.488082336265144,-0.00953319565535789,
0.517683952491609));
#31368=CARTESIAN_POINT('Ctrl Pts',(0.487629471678572,-0.185455272214093,
0.489281347254314));
#31369=CARTESIAN_POINT('Ctrl Pts',(0.487397673531982,-0.275065430413885,
0.463829888670926));
#31370=CARTESIAN_POINT('Ctrl Pts',(0.481096510297974,0.277761199726725,
0.473510370999757));
#31371=CARTESIAN_POINT('Ctrl Pts',(0.481560106591153,0.157531805062944,
0.507985809539987));
#31372=CARTESIAN_POINT('Ctrl Pts',(0.482123504397716,-0.00973590381621833,
0.528529637179682));
#31373=CARTESIAN_POINT('Ctrl Pts',(0.481444207517858,-0.187589153728891,
0.499366949904929));
#31374=CARTESIAN_POINT('Ctrl Pts',(0.481096510297973,-0.277761199726725,
0.473510370999756));
#31375=CARTESIAN_POINT('',(0.481671866090396,0.105573308103687,0.509780497494203));
#31376=CARTESIAN_POINT('',(0.484214864131698,-5.47020833232433E-5,0.511982600478171));
#31377=CARTESIAN_POINT('Ctrl Pts',(0.481669499211642,0.105481542418299,
0.509857066299145));
#31378=CARTESIAN_POINT('Ctrl Pts',(0.482460593225416,0.0888265354508503,
0.510603796014394));
#31379=CARTESIAN_POINT('Ctrl Pts',(0.483072065647681,0.0722091798017497,
0.511151842975794));
#31380=CARTESIAN_POINT('Ctrl Pts',(0.483497190939341,0.0555857456715263,
0.511504223118381));
#31381=CARTESIAN_POINT('Ctrl Pts',(0.483563383885825,0.0529974402769593,
0.511559089484552));
#31382=CARTESIAN_POINT('Ctrl Pts',(0.483625056117804,0.0504088952732917,
0.511609256996307));
#31383=CARTESIAN_POINT('Ctrl Pts',(0.4836821783703,0.047819849573354,0.511654784300019));
#31384=CARTESIAN_POINT('Ctrl Pts',(0.483917872556838,0.0371370947188088,
0.511842636150125));
#31385=CARTESIAN_POINT('Ctrl Pts',(0.484075802257484,0.0264653210899992,
0.511950708373913));
#31386=CARTESIAN_POINT('Ctrl Pts',(0.484155071769149,0.0157888211313803,
0.511984934956568));
#31387=CARTESIAN_POINT('Ctrl Pts',(0.484194291677581,0.0105064453231446,
0.512001869127216));
#31388=CARTESIAN_POINT('Ctrl Pts',(0.48421423214258,0.00522594818450658,
0.512000762646226));
#31389=CARTESIAN_POINT('Ctrl Pts',(0.484214864131698,-5.47020833232433E-5,
0.511982600478171));
#31390=CARTESIAN_POINT('',(0.481681895506807,-0.105694312340346,0.509518232484153));
#31391=CARTESIAN_POINT('Ctrl Pts',(0.484214864131698,-5.47020833232433E-5,
0.511982600478171));
#31392=CARTESIAN_POINT('Ctrl Pts',(0.484215270731505,-0.00346871674032279,
0.511970861826781));
#31393=CARTESIAN_POINT('Ctrl Pts',(0.484207605431539,-0.00688277797801751,
0.511951999455987));
#31394=CARTESIAN_POINT('Ctrl Pts',(0.484191857341194,-0.0102974597917216,
0.511926310507199));
#31395=CARTESIAN_POINT('Ctrl Pts',(0.484150901779444,-0.0191779150605256,
0.511859502068503));
#31396=CARTESIAN_POINT('Ctrl Pts',(0.484055314691237,-0.0280541644854541,
0.511746554850449));
#31397=CARTESIAN_POINT('Ctrl Pts',(0.483905243422272,-0.0369355028308617,
0.511593354983391));
#31398=CARTESIAN_POINT('Ctrl Pts',(0.483887560906102,-0.0379819683534304,
0.511575303832461));
#31399=CARTESIAN_POINT('Ctrl Pts',(0.483869121649569,-0.0390285027730886,
0.511556694950178));
#31400=CARTESIAN_POINT('Ctrl Pts',(0.483849926346507,-0.0400751201476585,
0.51153751894854));
#31401=CARTESIAN_POINT('Ctrl Pts',(0.483541868042211,-0.0568718944734031,
0.511229770405657));
#31402=CARTESIAN_POINT('Ctrl Pts',(0.483039907069928,-0.0736508998392528,
0.510775123483089));
#31403=CARTESIAN_POINT('Ctrl Pts',(0.482350711259662,-0.0904666554307169,
0.510143705463836));
#31404=CARTESIAN_POINT('Ctrl Pts',(0.482144613787803,-0.0954952476873488,
0.50995488589251));
#31405=CARTESIAN_POINT('Ctrl Pts',(0.481921888290475,-0.100524263582078,
0.509750479628641));
#31406=CARTESIAN_POINT('Ctrl Pts',(0.481682776226655,-0.10555484479313,
0.509530050599285));
#31407=CARTESIAN_POINT('Ctrl Pts',(0.481682776226651,-0.105554844794933,
0.509530050599066));
#31408=CARTESIAN_POINT('Ctrl Pts',(0.481553507568566,-0.158892946912007,
0.503053570640112));
#31409=CARTESIAN_POINT('Ctrl Pts',(0.481338736582444,-0.214942061649024,
0.491523580997232));
#31410=CARTESIAN_POINT('Ctrl Pts',(0.481096510297973,-0.277761199726725,
0.473510370999756));
#31411=CARTESIAN_POINT('Ctrl Pts',(0.5,-0.267674925037459,0.445024048994026));
#31412=CARTESIAN_POINT('Ctrl Pts',(0.5,-0.180075676750169,0.469283396273207));
#31413=CARTESIAN_POINT('Ctrl Pts',(0.5,-0.00916398135954615,0.495845869769614));
#31414=CARTESIAN_POINT('Ctrl Pts',(0.5,0.150652619934028,0.477444053637933));
#31415=CARTESIAN_POINT('Ctrl Pts',(0.5,0.267674912507086,0.445024157409761));
#31416=CARTESIAN_POINT('Ctrl Pts',(0.481096510297974,0.277761199726725,
0.473510370999757));
#31417=CARTESIAN_POINT('Ctrl Pts',(0.481338736582444,0.214942061649024,
0.491523580997232));
#31418=CARTESIAN_POINT('Ctrl Pts',(0.481542291138614,0.158851785396327,
0.503329833692243));
#31419=CARTESIAN_POINT('Ctrl Pts',(0.481669499211638,0.105481542420091,
0.509857066298925));
#31420=CARTESIAN_POINT('Origin',(0.490906733260264,0.283425134594813,0.));
#31421=CARTESIAN_POINT('',(0.5,0.267675134594813,0.0531981726275096));
#31422=CARTESIAN_POINT('',(0.481813466520527,0.299175134594813,0.0531981726275097));
#31423=CARTESIAN_POINT('Ctrl Pts',(0.5,0.267675134594813,0.0531981726275096));
#31424=CARTESIAN_POINT('Ctrl Pts',(0.490906733260264,0.283425134594813,
0.0528614692578827));
#31425=CARTESIAN_POINT('Ctrl Pts',(0.481813466520527,0.299175134594813,
0.0531981726275097));
#31426=CARTESIAN_POINT('',(0.481813466520527,0.299175134594813,0.));
#31427=CARTESIAN_POINT('',(0.5,0.267675134594813,0.));
#31428=CARTESIAN_POINT('Origin',(-1.37043154602168E-16,-0.566850269189626,
0.));
#31429=CARTESIAN_POINT('',(-0.0181865334794733,-0.566850269189626,0.0531981726275096));
#31430=CARTESIAN_POINT('',(0.018186533479473,-0.566850269189626,0.0531981726275097));
#31431=CARTESIAN_POINT('Ctrl Pts',(-0.0181865334794733,-0.566850269189626,
0.0531981726275096));
#31432=CARTESIAN_POINT('Ctrl Pts',(-9.71445146547012E-17,-0.566850269189626,
0.0528614692578828));
#31433=CARTESIAN_POINT('Ctrl Pts',(0.018186533479473,-0.566850269189626,
0.0531981726275097));
#31434=CARTESIAN_POINT('',(0.018186533479473,-0.566850269189626,0.));
#31435=CARTESIAN_POINT('',(-0.0181865334794733,-0.566850269189626,0.));
#31436=CARTESIAN_POINT('Ctrl Pts',(0.483544441026,-0.298175755998118,0.444468924013264));
#31437=CARTESIAN_POINT('Ctrl Pts',(0.406912985802199,-0.342418947299972,
0.469110141953084));
#31438=CARTESIAN_POINT('Ctrl Pts',(0.257908341391985,-0.428446818860714,
0.495972649874704));
#31439=CARTESIAN_POINT('Ctrl Pts',(0.118630832605733,-0.508858726050517,
0.477323881266358));
#31440=CARTESIAN_POINT('Ctrl Pts',(0.0164555589739991,-0.567849647786322,
0.444468924013264));
#31441=CARTESIAN_POINT('Ctrl Pts',(0.482728464116658,-0.291370903907653,
0.454149406342095));
#31442=CARTESIAN_POINT('Ctrl Pts',(0.405668349322323,-0.335995410650277,
0.479195744603699));
#31443=CARTESIAN_POINT('Ctrl Pts',(0.255104666887408,-0.42318499384238,
0.506818674741198));
#31444=CARTESIAN_POINT('Ctrl Pts',(0.113871724472837,-0.504508880129862,
0.487544524024234));
#31445=CARTESIAN_POINT('Ctrl Pts',(0.0109703726493327,-0.563740565008698,
0.454149406342095));
#31446=CARTESIAN_POINT('Ctrl Pts',(0.481912487207315,-0.284566051817189,
0.463829888670926));
#31447=CARTESIAN_POINT('Ctrl Pts',(0.404423712842447,-0.329571874000583,
0.489281347254314));
#31448=CARTESIAN_POINT('Ctrl Pts',(0.252300992382831,-0.417923168824047,
0.517664699607693));
#31449=CARTESIAN_POINT('Ctrl Pts',(0.109112616339942,-0.500159034209208,
0.49776516678211));
#31450=CARTESIAN_POINT('Ctrl Pts',(0.00548518632466623,-0.559631482231073,
0.463829888670926));
#31451=CARTESIAN_POINT('Ctrl Pts',(0.481096510297973,-0.277761199726725,
0.473510370999757));
#31452=CARTESIAN_POINT('Ctrl Pts',(0.403179076362571,-0.323148337350888,
0.499366949904929));
#31453=CARTESIAN_POINT('Ctrl Pts',(0.249497317878254,-0.412661343805714,
0.528510724474188));
#31454=CARTESIAN_POINT('Ctrl Pts',(0.104353508207047,-0.495809188288553,
0.507985809539986));
#31455=CARTESIAN_POINT('Ctrl Pts',(-1.94289029309402E-16,-0.555522399453449,
0.473510370999756));
#31456=CARTESIAN_POINT('',(0.332273583321351,-0.364361108482647,0.509521990816293));
#31457=CARTESIAN_POINT('',(0.14940638780266,-0.469927086065317,0.509774885821586));
#31458=CARTESIAN_POINT('Ctrl Pts',(0.332255993860884,-0.364371421655637,
0.50952333865621));
#31459=CARTESIAN_POINT('Ctrl Pts',(0.318279946918772,-0.373351253352252,
0.510249567790544));
#31460=CARTESIAN_POINT('Ctrl Pts',(0.30424598820164,-0.382157469729392,
0.510799578547912));
#31461=CARTESIAN_POINT('Ctrl Pts',(0.290111717192956,-0.390806403397131,
0.511195921402451));
#31462=CARTESIAN_POINT('Ctrl Pts',(0.28786005191306,-0.392184224979568,
0.511259060947741));
#31463=CARTESIAN_POINT('Ctrl Pts',(0.285605756140875,-0.393558099738538,
0.51131834900263));
#31464=CARTESIAN_POINT('Ctrl Pts',(0.283348567387484,-0.394928140744567,
0.51137392807787));
#31465=CARTESIAN_POINT('Ctrl Pts',(0.28021673730573,-0.396829060917713,
0.511451043569204));
#31466=CARTESIAN_POINT('Ctrl Pts',(0.277081273935522,-0.39872143776643,
0.511520951504387));
#31467=CARTESIAN_POINT('Ctrl Pts',(0.273941641913878,-0.400605537752241,
0.511584044834109));
#31468=CARTESIAN_POINT('Ctrl Pts',(0.267927330155411,-0.40421473928308,
0.511704907072807));
#31469=CARTESIAN_POINT('Ctrl Pts',(0.261897755700506,-0.407793556450531,
0.511800747922414));
#31470=CARTESIAN_POINT('Ctrl Pts',(0.255848830663054,-0.411344203910501,
0.51186864047409));
#31471=CARTESIAN_POINT('Ctrl Pts',(0.248348767769807,-0.415746652130085,
0.51195282045721));
#31472=CARTESIAN_POINT('Ctrl Pts',(0.240826093245984,-0.420101623101487,
0.511993883112245));
#31473=CARTESIAN_POINT('Ctrl Pts',(0.23327317900701,-0.42441364010989,0.511986957182665));
#31474=CARTESIAN_POINT('Ctrl Pts',(0.224651569134172,-0.429335783700461,
0.511979051272316));
#31475=CARTESIAN_POINT('Ctrl Pts',(0.215999456170051,-0.434196874243189,
0.511908560978458));
#31476=CARTESIAN_POINT('Ctrl Pts',(0.207306027932593,-0.43900385613391,
0.511770158465886));
#31477=CARTESIAN_POINT('Ctrl Pts',(0.192599818167027,-0.447135571504794,
0.511536030303051));
#31478=CARTESIAN_POINT('Ctrl Pts',(0.177810169615715,-0.455093185534589,
0.511107142930624));
#31479=CARTESIAN_POINT('Ctrl Pts',(0.162894469075872,-0.462908436068353,
0.510473800924483));
#31480=CARTESIAN_POINT('Ctrl Pts',(0.158434070265442,-0.465245512633472,
0.510284406003122));
#31481=CARTESIAN_POINT('Ctrl Pts',(0.153964937425981,-0.467568528701822,
0.510076948258664));
#31482=CARTESIAN_POINT('Ctrl Pts',(0.149486235114913,-0.469878234401733,
0.509851518489553));
#31483=CARTESIAN_POINT('Ctrl Pts',(0.149486235113333,-0.469878234402641,
0.50985151848933));
#31484=CARTESIAN_POINT('Ctrl Pts',(0.10320209198028,-0.496453452351217,
0.503326883310332));
#31485=CARTESIAN_POINT('Ctrl Pts',(0.054524082561366,-0.524322604530415,
0.491523580997232));
#31486=CARTESIAN_POINT('Ctrl Pts',(-1.94289029309402E-16,-0.555522399453449,
0.473510370999756));
#31487=CARTESIAN_POINT('Ctrl Pts',(0.018186726001538,-0.56685015803696,
0.44502415632149));
#31488=CARTESIAN_POINT('Ctrl Pts',(0.119531026231088,-0.508338999018595,
0.47744392523402));
#31489=CARTESIAN_POINT('Ctrl Pts',(0.257939671025404,-0.428428730688425,
0.495826064932766));
#31490=CARTESIAN_POINT('Ctrl Pts',(0.405950132909958,-0.342974850676498,
0.4692832678693));
#31491=CARTESIAN_POINT('Ctrl Pts',(0.481813285289659,-0.299175239228503,
0.445024047543947));
#31492=CARTESIAN_POINT('Ctrl Pts',(0.481096510297973,-0.277761199726725,
0.473510370999757));
#31493=CARTESIAN_POINT('Ctrl Pts',(0.426814654021077,-0.309380542881391,
0.491523580997232));
#31494=CARTESIAN_POINT('Ctrl Pts',(0.378382919626527,-0.337590700753812,
0.503049636797564));
#31495=CARTESIAN_POINT('Ctrl Pts',(0.332255993862453,-0.364371421654726,
0.50952333865599));
#31496=CARTESIAN_POINT('Origin',(0.490906733260263,-0.283425134594813,0.));
#31497=CARTESIAN_POINT('',(0.481813466520527,-0.299175134594813,0.0531981726275097));
#31498=CARTESIAN_POINT('',(0.5,-0.267675134594813,0.0531981726275096));
#31499=CARTESIAN_POINT('Ctrl Pts',(0.481813466520527,-0.299175134594813,
0.0531981726275097));
#31500=CARTESIAN_POINT('Ctrl Pts',(0.490906733260263,-0.283425134594813,
0.0528614692578827));
#31501=CARTESIAN_POINT('Ctrl Pts',(0.5,-0.267675134594813,0.0531981726275096));
#31502=CARTESIAN_POINT('',(0.5,-0.267675134594813,0.));
#31503=CARTESIAN_POINT('',(0.481813466520527,-0.299175134594813,0.));
#31504=CARTESIAN_POINT('Origin',(0.5,0.288675134594813,0.));
#31505=CARTESIAN_POINT('Ctrl Pts',(0.481813466520527,0.299175134594813,
0.0531981726275097));
#31506=CARTESIAN_POINT('Ctrl Pts',(0.249999999999998,0.433012701892221,
-0.0197414764085334));
#31507=CARTESIAN_POINT('Ctrl Pts',(0.0181865334794731,0.566850269189626,
0.0531981726275097));
#31508=CARTESIAN_POINT('Origin',(0.5,-0.288675134594813,0.));
#31509=CARTESIAN_POINT('Ctrl Pts',(0.5,-0.267675134594813,0.0531981726275096));
#31510=CARTESIAN_POINT('Ctrl Pts',(0.5,1.72084568816899E-15,-0.0197414764085334));
#31511=CARTESIAN_POINT('Ctrl Pts',(0.5,0.267675134594813,0.0531981726275096));
#31512=CARTESIAN_POINT('Origin',(-1.06057523872491E-16,-0.577350269189626,
0.));
#31513=CARTESIAN_POINT('Ctrl Pts',(0.018186533479473,-0.566850269189626,
0.0531981726275097));
#31514=CARTESIAN_POINT('Ctrl Pts',(0.250000000000002,-0.433012701892218,
-0.0197414764085333));
#31515=CARTESIAN_POINT('Ctrl Pts',(0.481813466520527,-0.299175134594813,
0.0531981726275097));
#31516=CARTESIAN_POINT('Origin',(0.,0.,0.0439797344638712));
#31517=CARTESIAN_POINT('',(-0.475,-5.81707229594992E-17,-5.55111512312578E-17));
#31518=CARTESIAN_POINT('Origin',(0.,0.,0.));
#31519=CARTESIAN_POINT('',(-0.5,-9.83216870916981E-17,0.0144337567297442));
#31520=CARTESIAN_POINT('',(-0.551175134594813,-6.74994864351149E-17,0.0439797344638712));
#31521=CARTESIAN_POINT('Ctrl Pts',(-0.5,0.267675134594813,0.0531981726275097));
#31522=CARTESIAN_POINT('Ctrl Pts',(-0.5,0.125416837769224,0.0144337567297444));
#31523=CARTESIAN_POINT('Ctrl Pts',(-0.5,-1.35411034226029E-16,0.0144337567297442));
#31524=CARTESIAN_POINT('Ctrl Pts',(-0.0181865334794732,0.566850269189626,
0.0531981726275097));
#31525=CARTESIAN_POINT('Ctrl Pts',(-0.250000000000002,0.433012701892218,
-0.0197414764085335));
#31526=CARTESIAN_POINT('Ctrl Pts',(-0.481813466520527,0.299175134594813,
0.0531981726275096));
#31527=CARTESIAN_POINT('Ctrl Pts',(-0.481813466520527,-0.299175134594813,
0.0531981726275097));
#31528=CARTESIAN_POINT('Ctrl Pts',(-0.249999999999999,-0.43301270189222,
-0.0197414764085333));
#31529=CARTESIAN_POINT('Ctrl Pts',(-0.0181865334794733,-0.566850269189626,
0.0531981726275096));
#31530=CARTESIAN_POINT('Ctrl Pts',(-0.5,-1.35411034226029E-16,0.0144337567297442));
#31531=CARTESIAN_POINT('Ctrl Pts',(-0.5,-0.125416837769225,0.014433756729744));
#31532=CARTESIAN_POINT('Ctrl Pts',(-0.5,-0.267675134594813,0.0531981726275096));
#31533=CARTESIAN_POINT('Origin',(0.,0.,0.476020265536129));
#31534=CARTESIAN_POINT('Origin',(0.,-3.01989654804108E-17,0.5095));
#31535=CARTESIAN_POINT('Origin',(0.,0.,0.476020265536129));
#31536=CARTESIAN_POINT('Origin',(0.,-3.01989654804108E-17,0.5095));
#31537=CARTESIAN_POINT('Origin',(0.,0.,0.476020265536129));
#31538=CARTESIAN_POINT('Origin',(0.,-3.01989654804108E-17,0.5095));
#31539=CARTESIAN_POINT('Origin',(0.,0.,0.476020265536129));
#31540=CARTESIAN_POINT('Origin',(0.,-3.01989654804108E-17,0.5095));
#31541=CARTESIAN_POINT('Origin',(0.,0.,0.476020265536129));
#31542=CARTESIAN_POINT('Origin',(0.,-3.01989654804108E-17,0.5095));
#31543=CARTESIAN_POINT('Origin',(0.,0.,0.476020265536129));
#31544=CARTESIAN_POINT('Origin',(0.,-3.01989654804108E-17,0.5095));
#31545=CARTESIAN_POINT('Origin',(0.,-1.50994827402054E-17,0.51475));
#31546=CARTESIAN_POINT('',(0.454,-5.55989646812898E-17,0.52));
#31547=CARTESIAN_POINT('Origin',(0.,0.,0.52));
#31548=CARTESIAN_POINT('',(0.473593266739736,5.79984478210557E-17,0.51475));
#31549=CARTESIAN_POINT('Origin',(0.,0.,0.52));
#31550=CARTESIAN_POINT('',(-0.366,-4.48220728487931E-17,0.52));
#31551=CARTESIAN_POINT('Origin',(0.,0.,0.52));
#31552=CARTESIAN_POINT('Origin',(0.,-1.01079517131223E-17,0.512575378797541));
#31553=CARTESIAN_POINT('',(-0.330150757595083,6.16297582203915E-33,0.505150757595083));
#31554=CARTESIAN_POINT('Origin',(0.,-2.02159034262446E-17,0.505150757595083));
#31555=CARTESIAN_POINT('',(-0.348075378797541,2.24110364243966E-17,0.512575378797541));
#31556=CARTESIAN_POINT('Origin',(0.,0.,0.5));
#31557=CARTESIAN_POINT('',(-0.319849242404917,-7.83404701841776E-17,0.494849242404917));
#31558=CARTESIAN_POINT('',(-0.325,-3.9801020972289E-17,0.5));
#31559=CARTESIAN_POINT('Origin',(0.,-1.95851175460444E-17,0.494849242404917));
#31560=CARTESIAN_POINT('Origin',(0.,-9.7925587730222E-18,0.476924621202459));
#31561=CARTESIAN_POINT('',(-0.305,3.73517273739943E-17,0.459));
#31562=CARTESIAN_POINT('',(-0.312424621202459,-5.78460987790859E-17,0.476924621202459));
#31563=CARTESIAN_POINT('Origin',(0.,0.,0.459));
#31564=CARTESIAN_POINT('Origin',(0.,0.,0.));
#31565=CARTESIAN_POINT('',(-0.305,-3.73517273739943E-17,0.04));
#31566=CARTESIAN_POINT('',(-0.305,-3.73517273739943E-17,0.));
#31567=CARTESIAN_POINT('Origin',(0.,0.,0.04));
#31568=CARTESIAN_POINT('Origin',(0.,0.,0.02));
#31569=CARTESIAN_POINT('',(-0.345,4.22503145705837E-17,0.));
#31570=CARTESIAN_POINT('',(-0.325,-3.9801020972289E-17,0.02));
#31571=CARTESIAN_POINT('Origin',(0.,0.,0.));
#31572=CARTESIAN_POINT('Origin',(0.,0.,0.));
#31573=CARTESIAN_POINT('Origin',(-0.5,-0.288675134594813,0.));
#31574=CARTESIAN_POINT('Origin',(-0.5,0.288675134594813,0.));
#31575=CARTESIAN_POINT('Origin',(3.53525079574969E-17,0.577350269189626,
0.));
#31576=CARTESIAN_POINT('',(0.,0.,0.));
#31577=CARTESIAN_POINT('',(0.,0.,3.));
#31578=CARTESIAN_POINT('',(0.,0.,3.));
#31579=CARTESIAN_POINT('',(0.,-2.4980018054066E-16,3.));
#31580=CARTESIAN_POINT('',(0.,0.,3.));
#31581=CARTESIAN_POINT('',(0.,0.,3.));
#31582=CARTESIAN_POINT('',(0.,0.,3.));
#31583=CARTESIAN_POINT('',(3.46944695195361E-18,-4.33680868994199E-19,3.));
#31584=CARTESIAN_POINT('',(4.6,-2.6,1.));
#31585=CARTESIAN_POINT('',(4.6,2.6,1.));
#31586=CARTESIAN_POINT('',(4.6,2.76,1.));
#31587=CARTESIAN_POINT('',(0.,-6.66133814775094E-16,3.));
#31588=CARTESIAN_POINT('',(1.55307697353708E-30,6.66133814775094E-16,3.));
#31589=CARTESIAN_POINT('',(1.55307697353708E-30,6.66133814775094E-16,3.));
#31590=CARTESIAN_POINT('',(0.,0.,5.25));
#31591=CARTESIAN_POINT('',(0.,0.,3.));
#31592=CARTESIAN_POINT('',(2.25,0.,3.));
#31593=CARTESIAN_POINT('',(0.,0.,3.));
#31594=CARTESIAN_POINT('',(-2.25,0.,3.));
#31595=CARTESIAN_POINT('',(0.,-6.66133814775094E-16,3.));
#31596=CARTESIAN_POINT('',(1.55307697353708E-30,6.66133814775094E-16,3.));
#31597=CARTESIAN_POINT('',(0.,-6.66133814775094E-16,3.));
#31598=CARTESIAN_POINT('',(1.55307697353708E-30,6.66133814775094E-16,3.));
#31599=CARTESIAN_POINT('',(0.,0.,3.));
#31600=CARTESIAN_POINT('',(0.,-6.66133814775094E-16,3.));
#31601=CARTESIAN_POINT('',(0.,-4.71844785465691E-16,3.));
#31602=CARTESIAN_POINT('',(1.55307697353708E-30,6.66133814775094E-16,3.));
#31603=CARTESIAN_POINT('',(1.62908404247163E-30,4.71844785465692E-16,3.));
#31604=CARTESIAN_POINT('',(4.6,-2.6,7.75));
#31605=CARTESIAN_POINT('',(-4.6,-2.6,1.));
#31606=CARTESIAN_POINT('',(-4.6,-2.6,7.75));
#31607=CARTESIAN_POINT('',(4.6,2.6,7.75));
#31608=CARTESIAN_POINT('',(-4.6,2.6,1.));
#31609=CARTESIAN_POINT('',(-4.6,2.6,7.75));
#31610=CARTESIAN_POINT('',(4.6,2.76,7.75));
#31611=CARTESIAN_POINT('',(-4.6,2.76,1.));
#31612=CARTESIAN_POINT('',(-4.6,2.76,7.75));
#31613=UNCERTAINTY_MEASURE_WITH_UNIT(LENGTH_MEASURE(0.001),#31639,
'DISTANCE_ACCURACY_VALUE',
'Maximum model space distance between geometric entities at asserted c
onnectivities');
#31614=UNCERTAINTY_MEASURE_WITH_UNIT(LENGTH_MEASURE(0.001),#31639,
'DISTANCE_ACCURACY_VALUE',
'Maximum model space distance between geometric entities at asserted c
onnectivities');
#31615=UNCERTAINTY_MEASURE_WITH_UNIT(LENGTH_MEASURE(0.001),#31639,
'DISTANCE_ACCURACY_VALUE',
'Maximum model space distance between geometric entities at asserted c
onnectivities');
#31616=UNCERTAINTY_MEASURE_WITH_UNIT(LENGTH_MEASURE(0.001),#31639,
'DISTANCE_ACCURACY_VALUE',
'Maximum model space distance between geometric entities at asserted c
onnectivities');
#31617=UNCERTAINTY_MEASURE_WITH_UNIT(LENGTH_MEASURE(0.001),#31639,
'DISTANCE_ACCURACY_VALUE',
'Maximum model space distance between geometric entities at asserted c
onnectivities');
#31618=UNCERTAINTY_MEASURE_WITH_UNIT(LENGTH_MEASURE(0.001),#31639,
'DISTANCE_ACCURACY_VALUE',
'Maximum model space distance between geometric entities at asserted c
onnectivities');
#31619=UNCERTAINTY_MEASURE_WITH_UNIT(LENGTH_MEASURE(0.001),#31639,
'DISTANCE_ACCURACY_VALUE',
'Maximum model space distance between geometric entities at asserted c
onnectivities');
#31620=UNCERTAINTY_MEASURE_WITH_UNIT(LENGTH_MEASURE(0.001),#31639,
'DISTANCE_ACCURACY_VALUE',
'Maximum model space distance between geometric entities at asserted c
onnectivities');
#31621=UNCERTAINTY_MEASURE_WITH_UNIT(LENGTH_MEASURE(0.001),#31639,
'DISTANCE_ACCURACY_VALUE',
'Maximum model space distance between geometric entities at asserted c
onnectivities');
#31622=UNCERTAINTY_MEASURE_WITH_UNIT(LENGTH_MEASURE(0.001),#31639,
'DISTANCE_ACCURACY_VALUE',
'Maximum model space distance between geometric entities at asserted c
onnectivities');
#31623=UNCERTAINTY_MEASURE_WITH_UNIT(LENGTH_MEASURE(0.001),#31639,
'DISTANCE_ACCURACY_VALUE',
'Maximum model space distance between geometric entities at asserted c
onnectivities');
#31624=UNCERTAINTY_MEASURE_WITH_UNIT(LENGTH_MEASURE(0.001),#31639,
'DISTANCE_ACCURACY_VALUE',
'Maximum model space distance between geometric entities at asserted c
onnectivities');
#31625=UNCERTAINTY_MEASURE_WITH_UNIT(LENGTH_MEASURE(0.001),#31639,
'DISTANCE_ACCURACY_VALUE',
'Maximum model space distance between geometric entities at asserted c
onnectivities');
#31626=(
GEOMETRIC_REPRESENTATION_CONTEXT(3)
GLOBAL_UNCERTAINTY_ASSIGNED_CONTEXT((#31613))
GLOBAL_UNIT_ASSIGNED_CONTEXT((#31639,#31641,#31642))
REPRESENTATION_CONTEXT('','3D')
);
#31627=(
GEOMETRIC_REPRESENTATION_CONTEXT(3)
GLOBAL_UNCERTAINTY_ASSIGNED_CONTEXT((#31614))
GLOBAL_UNIT_ASSIGNED_CONTEXT((#31639,#31641,#31642))
REPRESENTATION_CONTEXT('','3D')
);
#31628=(
GEOMETRIC_REPRESENTATION_CONTEXT(3)
GLOBAL_UNCERTAINTY_ASSIGNED_CONTEXT((#31615))
GLOBAL_UNIT_ASSIGNED_CONTEXT((#31639,#31641,#31642))
REPRESENTATION_CONTEXT('','3D')
);
#31629=(
GEOMETRIC_REPRESENTATION_CONTEXT(3)
GLOBAL_UNCERTAINTY_ASSIGNED_CONTEXT((#31616))
GLOBAL_UNIT_ASSIGNED_CONTEXT((#31639,#31641,#31642))
REPRESENTATION_CONTEXT('','3D')
);
#31630=(
GEOMETRIC_REPRESENTATION_CONTEXT(3)
GLOBAL_UNCERTAINTY_ASSIGNED_CONTEXT((#31617))
GLOBAL_UNIT_ASSIGNED_CONTEXT((#31639,#31641,#31642))
REPRESENTATION_CONTEXT('','3D')
);
#31631=(
GEOMETRIC_REPRESENTATION_CONTEXT(3)
GLOBAL_UNCERTAINTY_ASSIGNED_CONTEXT((#31618))
GLOBAL_UNIT_ASSIGNED_CONTEXT((#31639,#31641,#31642))
REPRESENTATION_CONTEXT('','3D')
);
#31632=(
GEOMETRIC_REPRESENTATION_CONTEXT(3)
GLOBAL_UNCERTAINTY_ASSIGNED_CONTEXT((#31619))
GLOBAL_UNIT_ASSIGNED_CONTEXT((#31639,#31641,#31642))
REPRESENTATION_CONTEXT('','3D')
);
#31633=(
GEOMETRIC_REPRESENTATION_CONTEXT(3)
GLOBAL_UNCERTAINTY_ASSIGNED_CONTEXT((#31620))
GLOBAL_UNIT_ASSIGNED_CONTEXT((#31639,#31641,#31642))
REPRESENTATION_CONTEXT('','3D')
);
#31634=(
GEOMETRIC_REPRESENTATION_CONTEXT(3)
GLOBAL_UNCERTAINTY_ASSIGNED_CONTEXT((#31621))
GLOBAL_UNIT_ASSIGNED_CONTEXT((#31639,#31641,#31642))
REPRESENTATION_CONTEXT('','3D')
);
#31635=(
GEOMETRIC_REPRESENTATION_CONTEXT(3)
GLOBAL_UNCERTAINTY_ASSIGNED_CONTEXT((#31622))
GLOBAL_UNIT_ASSIGNED_CONTEXT((#31639,#31641,#31642))
REPRESENTATION_CONTEXT('','3D')
);
#31636=(
GEOMETRIC_REPRESENTATION_CONTEXT(3)
GLOBAL_UNCERTAINTY_ASSIGNED_CONTEXT((#31623))
GLOBAL_UNIT_ASSIGNED_CONTEXT((#31639,#31641,#31642))
REPRESENTATION_CONTEXT('','3D')
);
#31637=(
GEOMETRIC_REPRESENTATION_CONTEXT(3)
GLOBAL_UNCERTAINTY_ASSIGNED_CONTEXT((#31624))
GLOBAL_UNIT_ASSIGNED_CONTEXT((#31639,#31641,#31642))
REPRESENTATION_CONTEXT('','3D')
);
#31638=(
GEOMETRIC_REPRESENTATION_CONTEXT(3)
GLOBAL_UNCERTAINTY_ASSIGNED_CONTEXT((#31625))
GLOBAL_UNIT_ASSIGNED_CONTEXT((#31639,#31641,#31642))
REPRESENTATION_CONTEXT('','3D')
);
#31639=(
LENGTH_UNIT()
NAMED_UNIT(*)
SI_UNIT(.CENTI.,.METRE.)
);
#31640=(
LENGTH_UNIT()
NAMED_UNIT(*)
SI_UNIT($,.METRE.)
);
#31641=(
NAMED_UNIT(*)
PLANE_ANGLE_UNIT()
SI_UNIT($,.RADIAN.)
);
#31642=(
NAMED_UNIT(*)
SI_UNIT($,.STERADIAN.)
SOLID_ANGLE_UNIT()
);
#31643=SHAPE_DEFINITION_REPRESENTATION(#31655,#31704);
#31644=SHAPE_DEFINITION_REPRESENTATION(#31656,#31705);
#31645=SHAPE_DEFINITION_REPRESENTATION(#31657,#31706);
#31646=SHAPE_DEFINITION_REPRESENTATION(#31658,#31707);
#31647=SHAPE_DEFINITION_REPRESENTATION(#31659,#31708);
#31648=SHAPE_DEFINITION_REPRESENTATION(#31660,#31709);
#31649=SHAPE_DEFINITION_REPRESENTATION(#31661,#31710);
#31650=SHAPE_DEFINITION_REPRESENTATION(#31662,#31711);
#31651=SHAPE_DEFINITION_REPRESENTATION(#31663,#31712);
#31652=SHAPE_DEFINITION_REPRESENTATION(#31664,#31713);
#31653=SHAPE_DEFINITION_REPRESENTATION(#31665,#31714);
#31654=SHAPE_DEFINITION_REPRESENTATION(#31666,#31715);
#31655=PRODUCT_DEFINITION_SHAPE('',$,#31717);
#31656=PRODUCT_DEFINITION_SHAPE('',$,#31718);
#31657=PRODUCT_DEFINITION_SHAPE('',$,#31719);
#31658=PRODUCT_DEFINITION_SHAPE('',$,#31720);
#31659=PRODUCT_DEFINITION_SHAPE('',$,#31721);
#31660=PRODUCT_DEFINITION_SHAPE('',$,#31722);
#31661=PRODUCT_DEFINITION_SHAPE('',$,#31723);
#31662=PRODUCT_DEFINITION_SHAPE('',$,#31724);
#31663=PRODUCT_DEFINITION_SHAPE('',$,#31725);
#31664=PRODUCT_DEFINITION_SHAPE('',$,#31726);
#31665=PRODUCT_DEFINITION_SHAPE('',$,#31727);
#31666=PRODUCT_DEFINITION_SHAPE('',$,#31728);
#31667=PRODUCT_DEFINITION_SHAPE($,$,#122);
#31668=PRODUCT_DEFINITION_SHAPE($,$,#123);
#31669=PRODUCT_DEFINITION_SHAPE($,$,#124);
#31670=PRODUCT_DEFINITION_SHAPE($,$,#125);
#31671=PRODUCT_DEFINITION_SHAPE($,$,#126);
#31672=PRODUCT_DEFINITION_SHAPE($,$,#127);
#31673=PRODUCT_DEFINITION_SHAPE($,$,#128);
#31674=PRODUCT_DEFINITION_SHAPE($,$,#129);
#31675=PRODUCT_DEFINITION_SHAPE($,$,#130);
#31676=PRODUCT_DEFINITION_SHAPE($,$,#131);
#31677=PRODUCT_DEFINITION_SHAPE($,$,#132);
#31678=PRODUCT_DEFINITION_SHAPE($,$,#133);
#31679=PRODUCT_DEFINITION_SHAPE($,$,#134);
#31680=PRODUCT_DEFINITION_SHAPE($,$,#135);
#31681=PRODUCT_DEFINITION_SHAPE($,$,#136);
#31682=PRODUCT_DEFINITION_SHAPE($,$,#137);
#31683=PRODUCT_DEFINITION_SHAPE($,$,#138);
#31684=PRODUCT_DEFINITION_SHAPE($,$,#139);
#31685=PRODUCT_DEFINITION_SHAPE($,$,#140);
#31686=PRODUCT_DEFINITION_SHAPE($,$,#141);
#31687=PRODUCT_DEFINITION_SHAPE($,$,#142);
#31688=PRODUCT_DEFINITION_SHAPE($,$,#143);
#31689=PRODUCT_DEFINITION_SHAPE($,$,#144);
#31690=PRODUCT_DEFINITION_SHAPE($,$,#145);
#31691=PRODUCT_DEFINITION_SHAPE($,$,#146);
#31692=PRODUCT_DEFINITION_SHAPE($,$,#147);
#31693=PRODUCT_DEFINITION_SHAPE($,$,#148);
#31694=PRODUCT_DEFINITION_SHAPE($,$,#149);
#31695=PRODUCT_DEFINITION_SHAPE($,$,#150);
#31696=PRODUCT_DEFINITION_SHAPE($,$,#151);
#31697=PRODUCT_DEFINITION_SHAPE($,$,#152);
#31698=PRODUCT_DEFINITION_SHAPE($,$,#153);
#31699=PRODUCT_DEFINITION_SHAPE($,$,#154);
#31700=PRODUCT_DEFINITION_SHAPE($,$,#155);
#31701=PRODUCT_DEFINITION_SHAPE($,$,#156);
#31702=PRODUCT_DEFINITION_SHAPE($,$,#157);
#31703=PRODUCT_DEFINITION_SHAPE($,$,#158);
#31704=SHAPE_REPRESENTATION('',(#12613,#13583,#13584,#13585,#13586,#13587,
#13588,#13589,#13590,#13591,#13592,#13593,#13594,#13595,#13596,#13597,#13598,
#13599,#13600,#13601,#13602,#13603,#13604,#13605,#13606,#13607,#13608,#13609,
#13610,#13611,#13612,#13613,#13614,#13615,#13616,#13617,#13618,#13619),
#31626);
#31705=SHAPE_REPRESENTATION('',(#12614),#31627);
#31706=SHAPE_REPRESENTATION('',(#12776),#31628);
#31707=SHAPE_REPRESENTATION('',(#12865),#31629);
#31708=SHAPE_REPRESENTATION('',(#12900),#31630);
#31709=SHAPE_REPRESENTATION('',(#12986),#31631);
#31710=SHAPE_REPRESENTATION('',(#13096),#31632);
#31711=SHAPE_REPRESENTATION('',(#13105),#31633);
#31712=SHAPE_REPRESENTATION('',(#13136),#31634);
#31713=SHAPE_REPRESENTATION('',(#13175),#31635);
#31714=SHAPE_REPRESENTATION('',(#13515),#31636);
#31715=SHAPE_REPRESENTATION('',(#13535),#31637);
#31716=PRODUCT_DEFINITION_CONTEXT('part definition',#31754,'design');
#31717=PRODUCT_DEFINITION('2026-10-22-02-42-08-798','MAS-358',#31729,#31716);
#31718=PRODUCT_DEFINITION('2026-10-22-02-42-10-486',
'01_Aluminium_Gearbox_Frame_115x87.5x52',#31730,#31716);
#31719=PRODUCT_DEFINITION('2026-10-22-02-42-12-427',
'03_Spiral_Bevel_Pinion_m1.75_z20_LH_Input',#31731,#31716);
#31720=PRODUCT_DEFINITION('2026-10-22-02-42-12-024',
'02_Drive_Shaft_D10h6x92.8_Flats_Circlip_Groove',#31732,#31716);
#31721=PRODUCT_DEFINITION('2026-10-22-02-42-16-551',
'04_Spiral_Bevel_Side_Gear_m1.75_z20_RH_Output',#31733,#31716);
#31722=PRODUCT_DEFINITION('2026-10-22-02-42-20-042',
'05_Deep_Groove_Ball_Bearing_6000-ZZ_10x26x8',#31734,#31716);
#31723=PRODUCT_DEFINITION('2026-10-22-02-42-21-610',
'06_DIN_988_Shim_Ring_10x16x1.0',#31735,#31716);
#31724=PRODUCT_DEFINITION('2026-10-22-02-42-21-963',
'07_DIN_471_Retaining_Ring_10x1',#31736,#31716);
#31725=PRODUCT_DEFINITION('2026-10-22-02-42-23-427',
'08_ISO_4026_M4x5_Hex_Socket_Set_Screw_Flat_Point',#31737,#31716);
#31726=PRODUCT_DEFINITION('2026-10-22-02-42-24-626',
'09_ISO_4762_M6x60-8.8_Socket_Head_Cap_Screw',#31738,#31716);
#31727=PRODUCT_DEFINITION('2026-10-22-02-42-33-064',
'10_ISO_7089_Washer_6_200HV',#31739,#31716);
#31728=PRODUCT_DEFINITION('2026-10-22-02-42-33-605',
'11_ISO_4032_M6-8_Hex_Nut',#31740,#31716);
#31729=PRODUCT_DEFINITION_FORMATION('',$,#31756);
#31730=PRODUCT_DEFINITION_FORMATION('',$,#31757);
#31731=PRODUCT_DEFINITION_FORMATION('',$,#31758);
#31732=PRODUCT_DEFINITION_FORMATION('',$,#31759);
#31733=PRODUCT_DEFINITION_FORMATION('',$,#31760);
#31734=PRODUCT_DEFINITION_FORMATION('',$,#31761);
#31735=PRODUCT_DEFINITION_FORMATION('',$,#31762);
#31736=PRODUCT_DEFINITION_FORMATION('',$,#31763);
#31737=PRODUCT_DEFINITION_FORMATION('',$,#31764);
#31738=PRODUCT_DEFINITION_FORMATION('',$,#31765);
#31739=PRODUCT_DEFINITION_FORMATION('',$,#31766);
#31740=PRODUCT_DEFINITION_FORMATION('',$,#31767);
#31741=PRODUCT_RELATED_PRODUCT_CATEGORY('MAS-358','MAS-358',(#31756));
#31742=PRODUCT_RELATED_PRODUCT_CATEGORY(
'01_Aluminium_Gearbox_Frame_115x87.5x52',
'01_Aluminium_Gearbox_Frame_115x87.5x52',(#31757));
#31743=PRODUCT_RELATED_PRODUCT_CATEGORY(
'03_Spiral_Bevel_Pinion_m1.75_z20_LH_Input',
'03_Spiral_Bevel_Pinion_m1.75_z20_LH_Input',(#31758));
#31744=PRODUCT_RELATED_PRODUCT_CATEGORY(
'02_Drive_Shaft_D10h6x92.8_Flats_Circlip_Groove',
'02_Drive_Shaft_D10h6x92.8_Flats_Circlip_Groove',(#31759));
#31745=PRODUCT_RELATED_PRODUCT_CATEGORY(
'04_Spiral_Bevel_Side_Gear_m1.75_z20_RH_Output',
'04_Spiral_Bevel_Side_Gear_m1.75_z20_RH_Output',(#31760));
#31746=PRODUCT_RELATED_PRODUCT_CATEGORY(
'05_Deep_Groove_Ball_Bearing_6000-ZZ_10x26x8',
'05_Deep_Groove_Ball_Bearing_6000-ZZ_10x26x8',(#31761));
#31747=PRODUCT_RELATED_PRODUCT_CATEGORY(
'06_DIN_988_Shim_Ring_10x16x1.0','06_DIN_988_Shim_Ring_10x16x1.0',(#31762));
#31748=PRODUCT_RELATED_PRODUCT_CATEGORY(
'07_DIN_471_Retaining_Ring_10x1','07_DIN_471_Retaining_Ring_10x1',(#31763));
#31749=PRODUCT_RELATED_PRODUCT_CATEGORY(
'08_ISO_4026_M4x5_Hex_Socket_Set_Screw_Flat_Point',
'08_ISO_4026_M4x5_Hex_Socket_Set_Screw_Flat_Point',(#31764));
#31750=PRODUCT_RELATED_PRODUCT_CATEGORY(
'09_ISO_4762_M6x60-8.8_Socket_Head_Cap_Screw',
'09_ISO_4762_M6x60-8.8_Socket_Head_Cap_Screw',(#31765));
#31751=PRODUCT_RELATED_PRODUCT_CATEGORY('10_ISO_7089_Washer_6_200HV',
'10_ISO_7089_Washer_6_200HV',(#31766));
#31752=PRODUCT_RELATED_PRODUCT_CATEGORY('11_ISO_4032_M6-8_Hex_Nut',
'11_ISO_4032_M6-8_Hex_Nut',(#31767));
#31753=APPLICATION_PROTOCOL_DEFINITION('international standard',
'automotive_design',2009,#31754);
#31754=APPLICATION_CONTEXT(
'Core Data for Automotive Mechanical Design Process');
#31755=PRODUCT_CONTEXT('part definition',#31754,'mechanical');
#31756=PRODUCT('2026-10-22-02-42-08-798','MAS-358',$,(#31755));
#31757=PRODUCT('2026-10-22-02-42-10-486',
'01_Aluminium_Gearbox_Frame_115x87.5x52',$,(#31755));
#31758=PRODUCT('2026-10-22-02-42-12-427',
'03_Spiral_Bevel_Pinion_m1.75_z20_LH_Input',$,(#31755));
#31759=PRODUCT('2026-10-22-02-42-12-024',
'02_Drive_Shaft_D10h6x92.8_Flats_Circlip_Groove',$,(#31755));
#31760=PRODUCT('2026-10-22-02-42-16-551',
'04_Spiral_Bevel_Side_Gear_m1.75_z20_RH_Output',$,(#31755));
#31761=PRODUCT('2026-10-22-02-42-20-042',
'05_Deep_Groove_Ball_Bearing_6000-ZZ_10x26x8',$,(#31755));
#31762=PRODUCT('2026-10-22-02-42-21-610',
'06_DIN_988_Shim_Ring_10x16x1.0',$,(#31755));
#31763=PRODUCT('2026-10-22-02-42-21-963',
'07_DIN_471_Retaining_Ring_10x1',$,(#31755));
#31764=PRODUCT('2026-10-22-02-42-23-427',
'08_ISO_4026_M4x5_Hex_Socket_Set_Screw_Flat_Point',$,(#31755));
#31765=PRODUCT('2026-10-22-02-42-24-626',
'09_ISO_4762_M6x60-8.8_Socket_Head_Cap_Screw',$,(#31755));
#31766=PRODUCT('2026-10-22-02-42-33-064','10_ISO_7089_Washer_6_200HV',$,
(#31755));
#31767=PRODUCT('2026-10-22-02-42-33-605','11_ISO_4032_M6-8_Hex_Nut',$,(#31755));
#31768=PRESENTATION_STYLE_ASSIGNMENT((#31773));
#31769=PRESENTATION_STYLE_ASSIGNMENT((#31774));
#31770=PRESENTATION_STYLE_ASSIGNMENT((#31775));
#31771=PRESENTATION_STYLE_ASSIGNMENT((#31776));
#31772=PRESENTATION_STYLE_ASSIGNMENT((#31777));
#31773=SURFACE_STYLE_USAGE(.BOTH.,#31778);
#31774=SURFACE_STYLE_USAGE(.BOTH.,#31779);
#31775=SURFACE_STYLE_USAGE(.BOTH.,#31780);
#31776=SURFACE_STYLE_USAGE(.BOTH.,#31781);
#31777=SURFACE_STYLE_USAGE(.BOTH.,#31782);
#31778=SURFACE_SIDE_STYLE('',(#31783));
#31779=SURFACE_SIDE_STYLE('',(#31784));
#31780=SURFACE_SIDE_STYLE('',(#31785));
#31781=SURFACE_SIDE_STYLE('',(#31786));
#31782=SURFACE_SIDE_STYLE('',(#31787));
#31783=SURFACE_STYLE_FILL_AREA(#31788);
#31784=SURFACE_STYLE_FILL_AREA(#31789);
#31785=SURFACE_STYLE_FILL_AREA(#31790);
#31786=SURFACE_STYLE_FILL_AREA(#31791);
#31787=SURFACE_STYLE_FILL_AREA(#31792);
#31788=FILL_AREA_STYLE('Steel - Satin',(#31793));
#31789=FILL_AREA_STYLE('Satin_Aluminium_ADB4BA',(#31794));
#31790=FILL_AREA_STYLE('Gunmetal_Silver_50565D',(#31795));
#31791=FILL_AREA_STYLE('Polished_Stainless_Steel_D6D9DC',(#31796));
#31792=FILL_AREA_STYLE('Brushed_Titanium_Silver_8C9298',(#31797));
#31793=FILL_AREA_STYLE_COLOUR('Steel - Satin',#31798);
#31794=FILL_AREA_STYLE_COLOUR('Satin_Aluminium_ADB4BA',#31799);
#31795=FILL_AREA_STYLE_COLOUR('Gunmetal_Silver_50565D',#31800);
#31796=FILL_AREA_STYLE_COLOUR('Polished_Stainless_Steel_D6D9DC',#31801);
#31797=FILL_AREA_STYLE_COLOUR('Brushed_Titanium_Silver_8C9298',#31802);
#31798=COLOUR_RGB('Steel - Satin',0.627450980392157,0.627450980392157,0.627450980392157);
#31799=COLOUR_RGB('Satin_Aluminium_ADB4BA',0.67843137254902,0.705882352941177,
0.729411764705882);
#31800=COLOUR_RGB('Gunmetal_Silver_50565D',0.313725490196078,0.337254901960784,
0.364705882352941);
#31801=COLOUR_RGB('Polished_Stainless_Steel_D6D9DC',0.83921568627451,0.850980392156863,
0.862745098039216);
#31802=COLOUR_RGB('Brushed_Titanium_Silver_8C9298',0.549019607843137,0.572549019607843,
0.596078431372549);
#31803=COLOUR_RGB('Dark Blue',0.08,0.2,0.34);
#31804=FILL_AREA_STYLE_COLOUR('',#31803);
#31805=FILL_AREA_STYLE('',(#31804));
#31806=SURFACE_STYLE_FILL_AREA(#31805);
#31807=SURFACE_SIDE_STYLE('',(#31806));
#31808=SURFACE_STYLE_USAGE(.BOTH.,#31807);
#31809=PRESENTATION_STYLE_ASSIGNMENT((#31808));
#31810=COLOUR_RGB('Light Blue',0.38,0.62,0.78);
#31811=FILL_AREA_STYLE_COLOUR('',#31810);
#31812=FILL_AREA_STYLE('',(#31811));
#31813=SURFACE_STYLE_FILL_AREA(#31812);
#31814=SURFACE_SIDE_STYLE('',(#31813));
#31815=SURFACE_STYLE_USAGE(.BOTH.,#31814);
#31816=PRESENTATION_STYLE_ASSIGNMENT((#31815));
#31817=COLOUR_RGB('Sky Blue',0.24,0.69,0.87);
#31818=FILL_AREA_STYLE_COLOUR('',#31817);
#31819=FILL_AREA_STYLE('',(#31818));
#31820=SURFACE_STYLE_FILL_AREA(#31819);
#31821=SURFACE_SIDE_STYLE('',(#31820));
#31822=SURFACE_STYLE_USAGE(.BOTH.,#31821);
#31823=PRESENTATION_STYLE_ASSIGNMENT((#31822));
#31824=COLOUR_RGB('Grey',0.48,0.52,0.57);
#31825=FILL_AREA_STYLE_COLOUR('',#31824);
#31826=FILL_AREA_STYLE('',(#31825));
#31827=SURFACE_STYLE_FILL_AREA(#31826);
#31828=SURFACE_SIDE_STYLE('',(#31827));
#31829=SURFACE_STYLE_USAGE(.BOTH.,#31828);
#31830=PRESENTATION_STYLE_ASSIGNMENT((#31829));
#31831=COLOUR_RGB('Black',0.12,0.14,0.17);
#31832=FILL_AREA_STYLE_COLOUR('',#31831);
#31833=FILL_AREA_STYLE('',(#31832));
#31834=SURFACE_STYLE_FILL_AREA(#31833);
#31835=SURFACE_SIDE_STYLE('',(#31834));
#31836=SURFACE_STYLE_USAGE(.BOTH.,#31835);
#31837=PRESENTATION_STYLE_ASSIGNMENT((#31836));
#31838=COLOUR_RGB('Off White',0.89,0.88,0.83);
#31839=FILL_AREA_STYLE_COLOUR('',#31838);
#31840=FILL_AREA_STYLE('',(#31839));
#31841=SURFACE_STYLE_FILL_AREA(#31840);
#31842=SURFACE_SIDE_STYLE('',(#31841));
#31843=SURFACE_STYLE_USAGE(.BOTH.,#31842);
#31844=PRESENTATION_STYLE_ASSIGNMENT((#31843));
ENDSEC;
END-ISO-10303-21;
